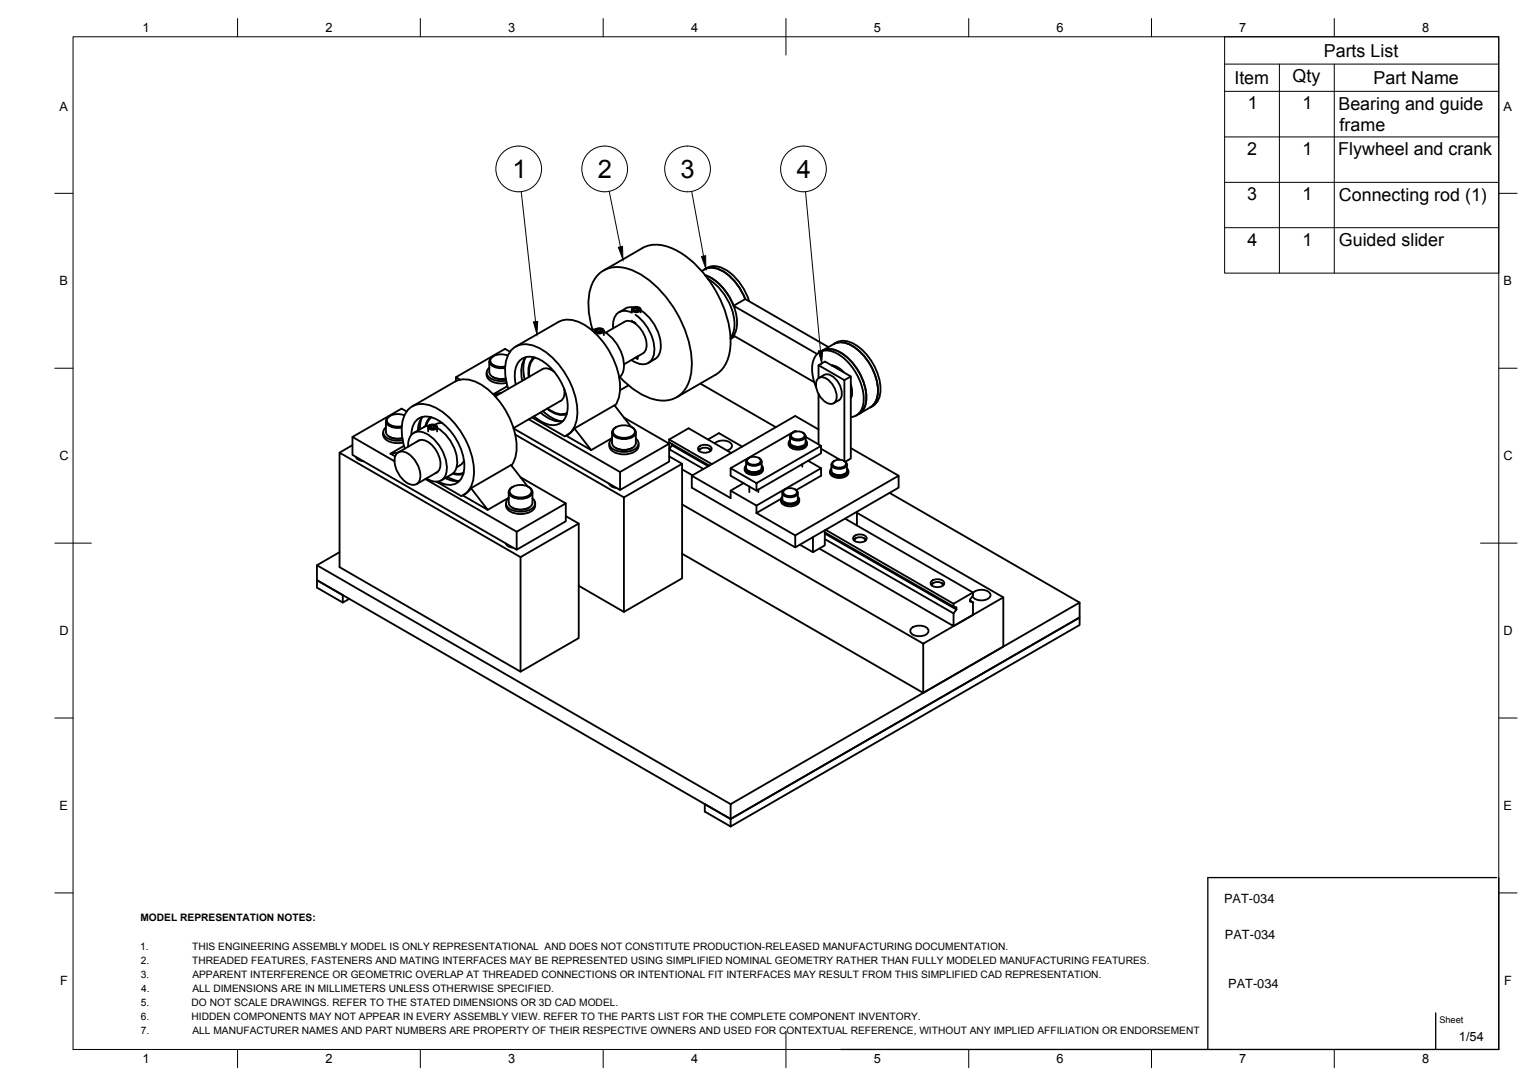
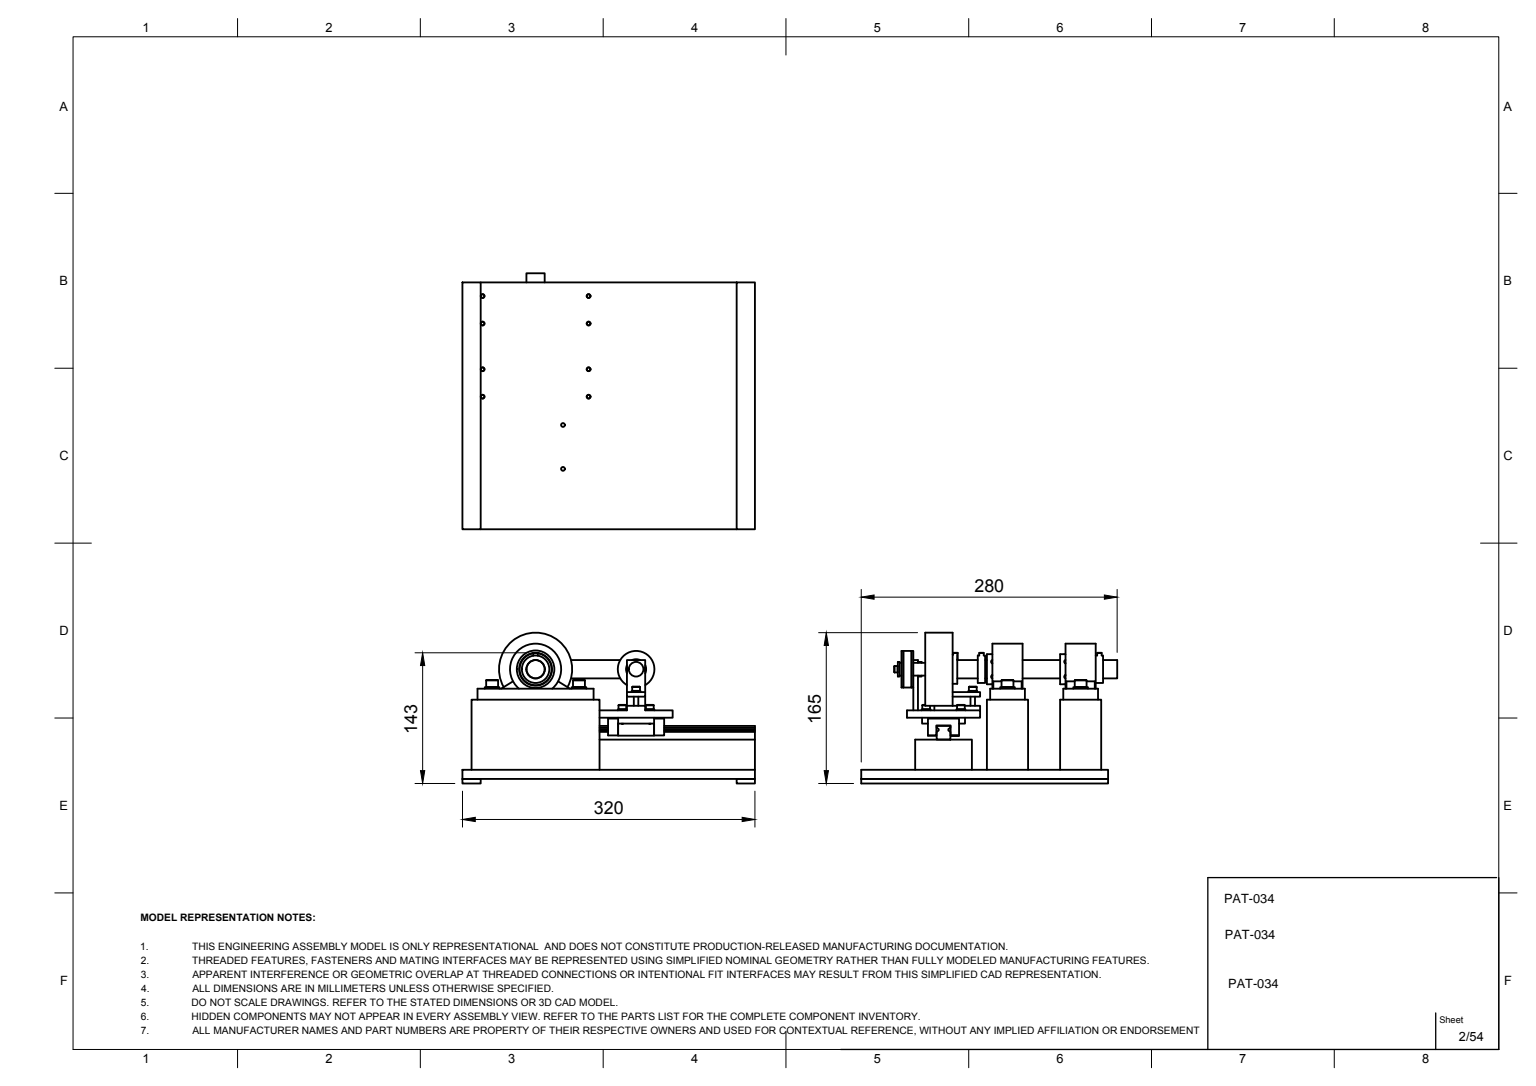
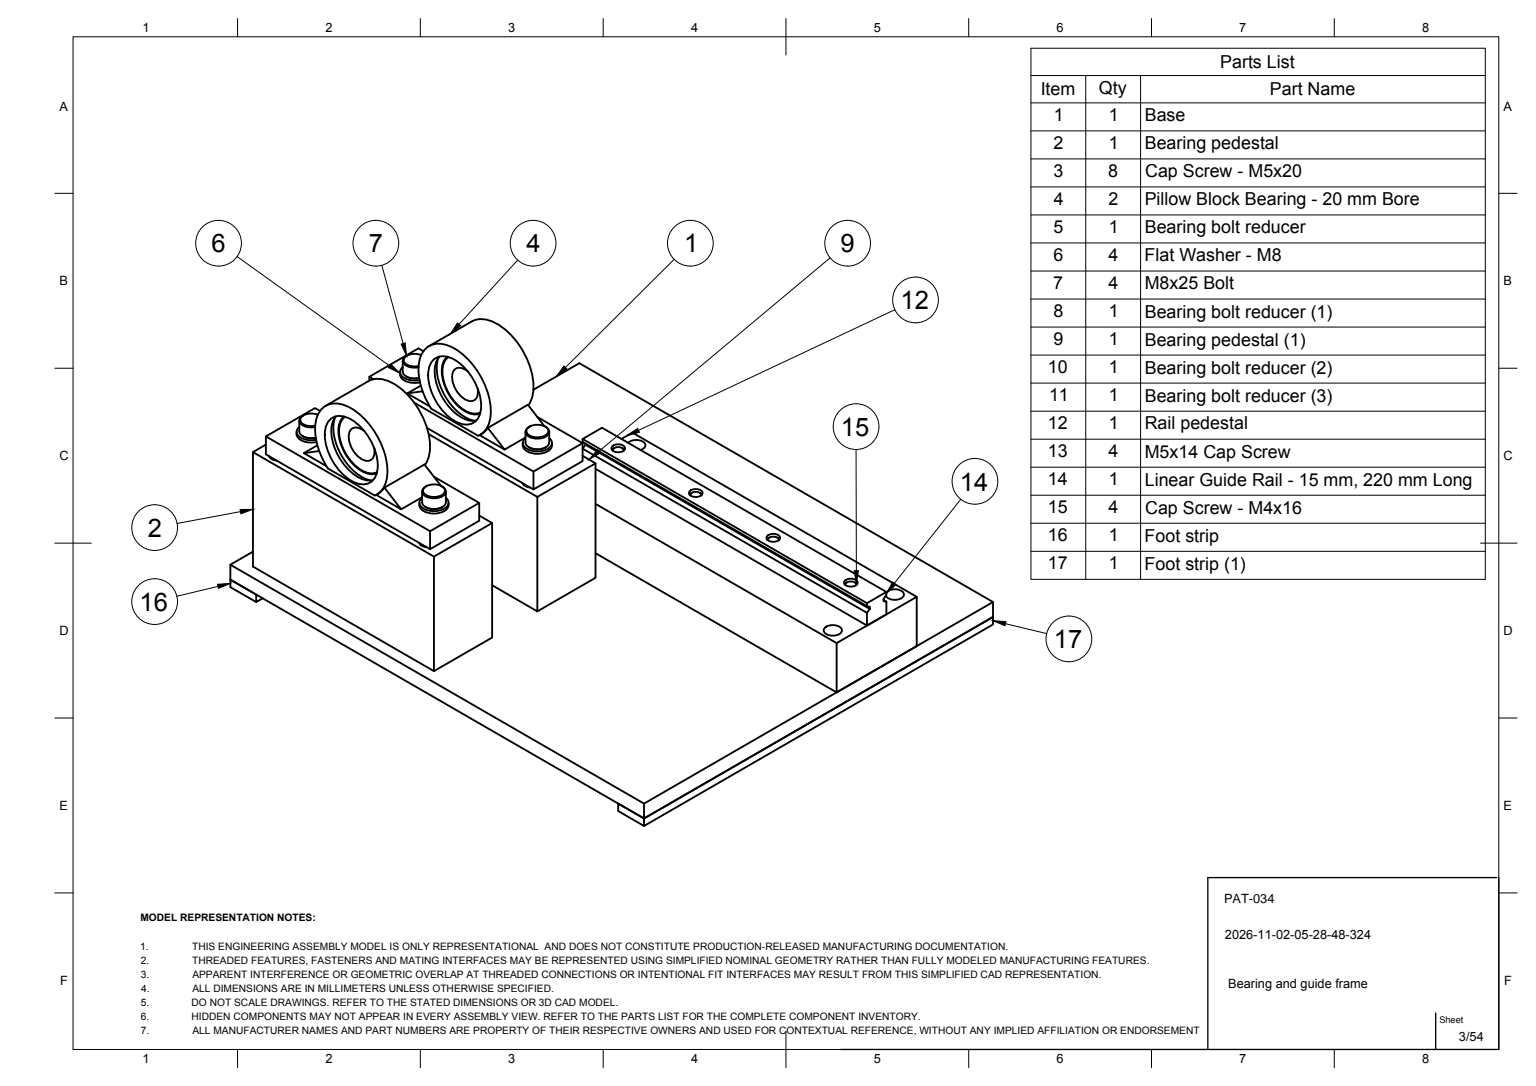
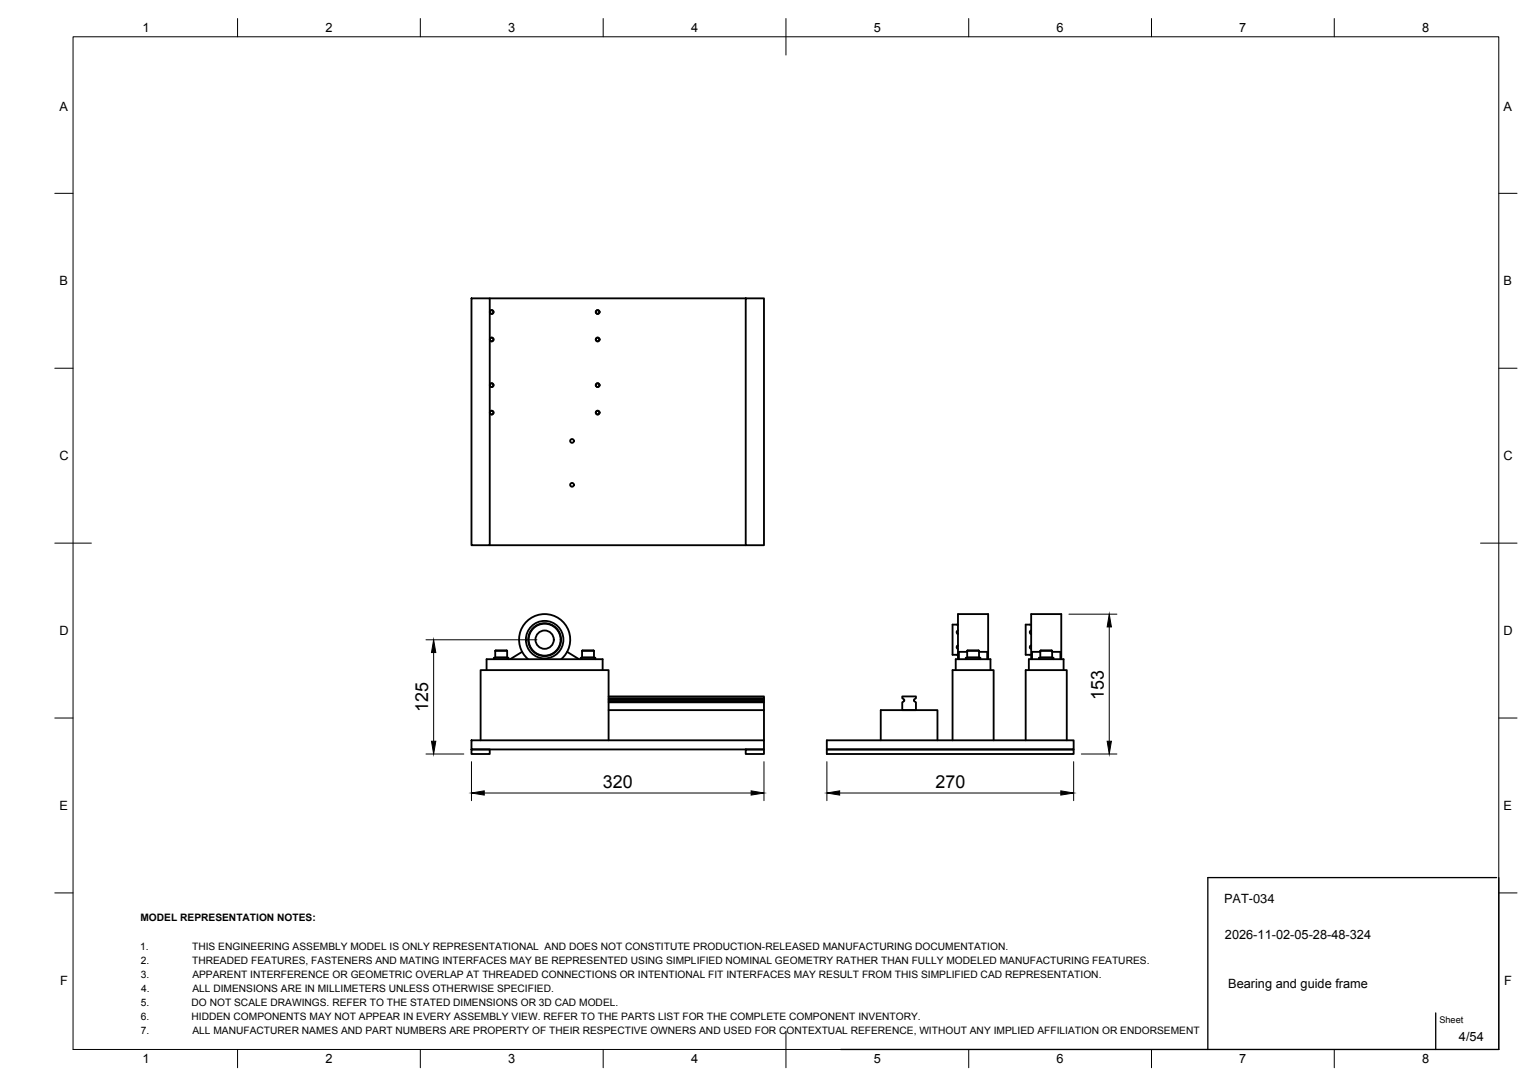
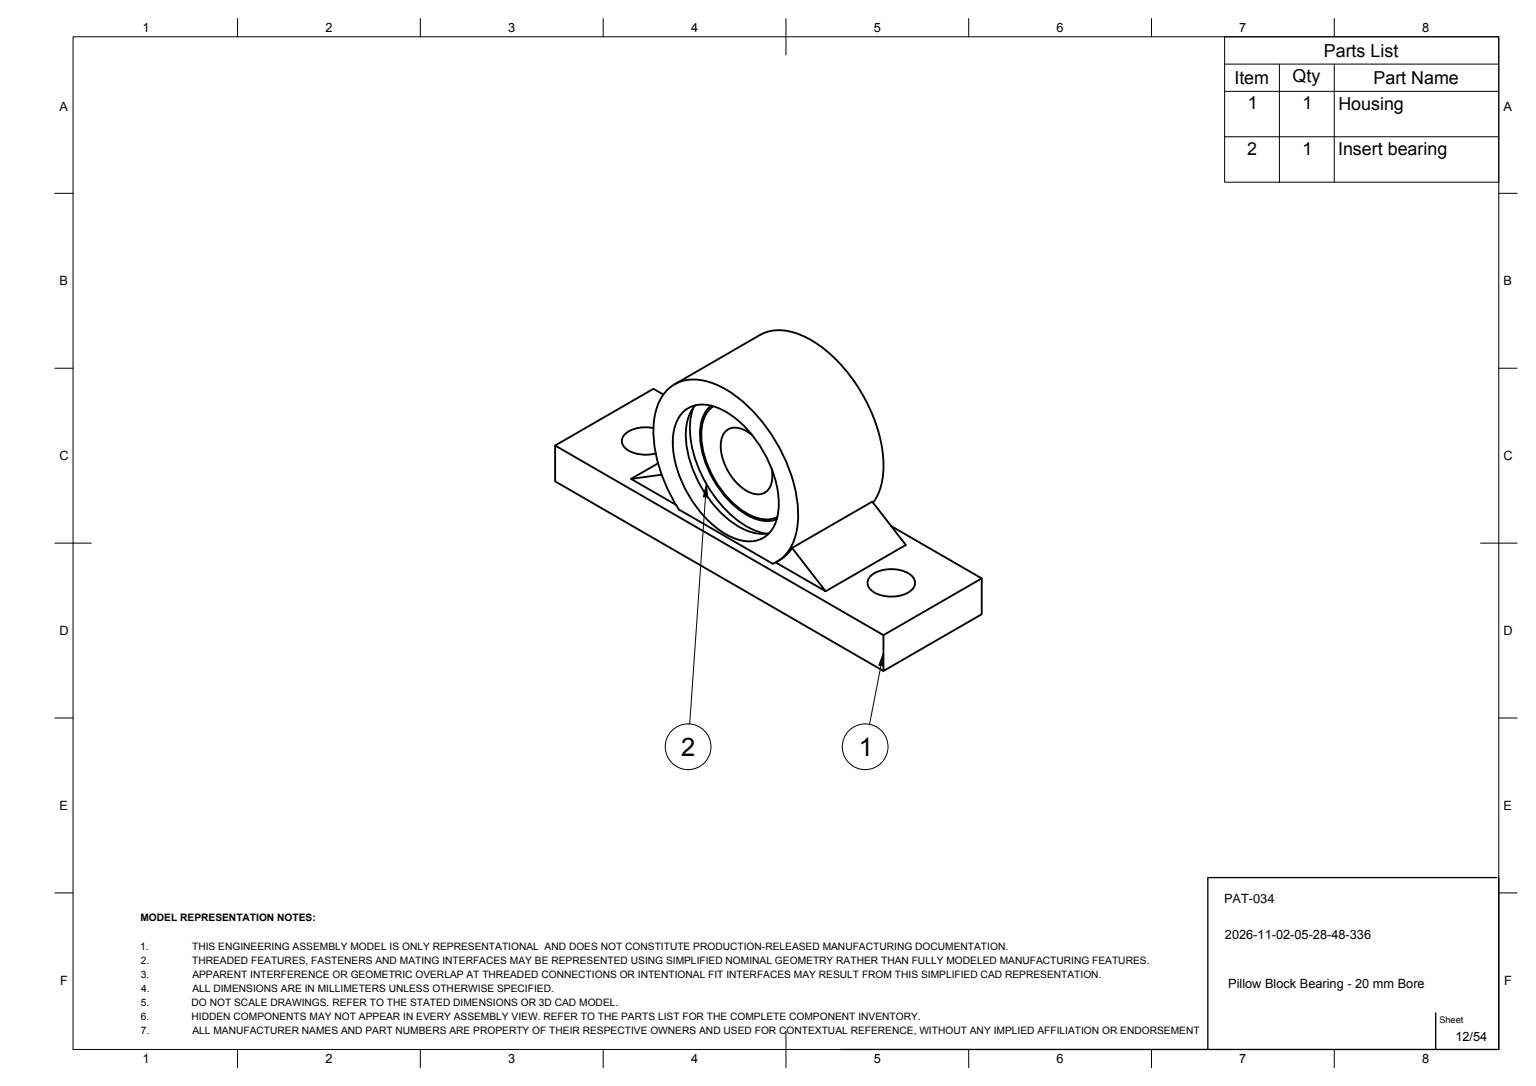
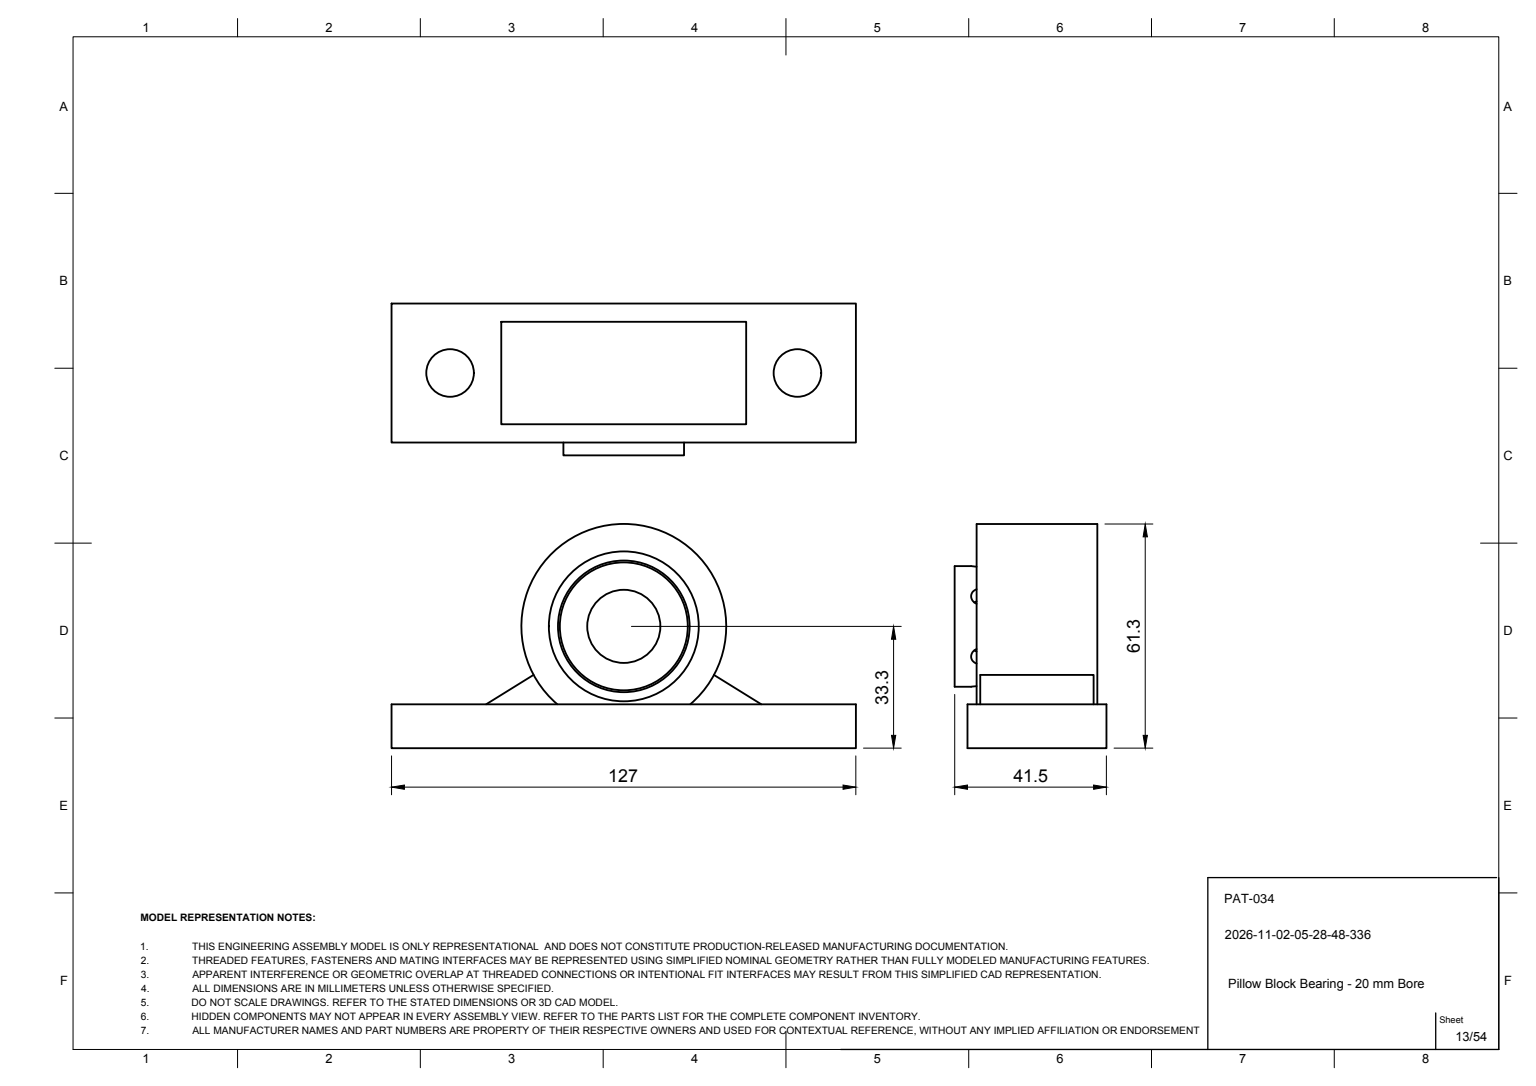
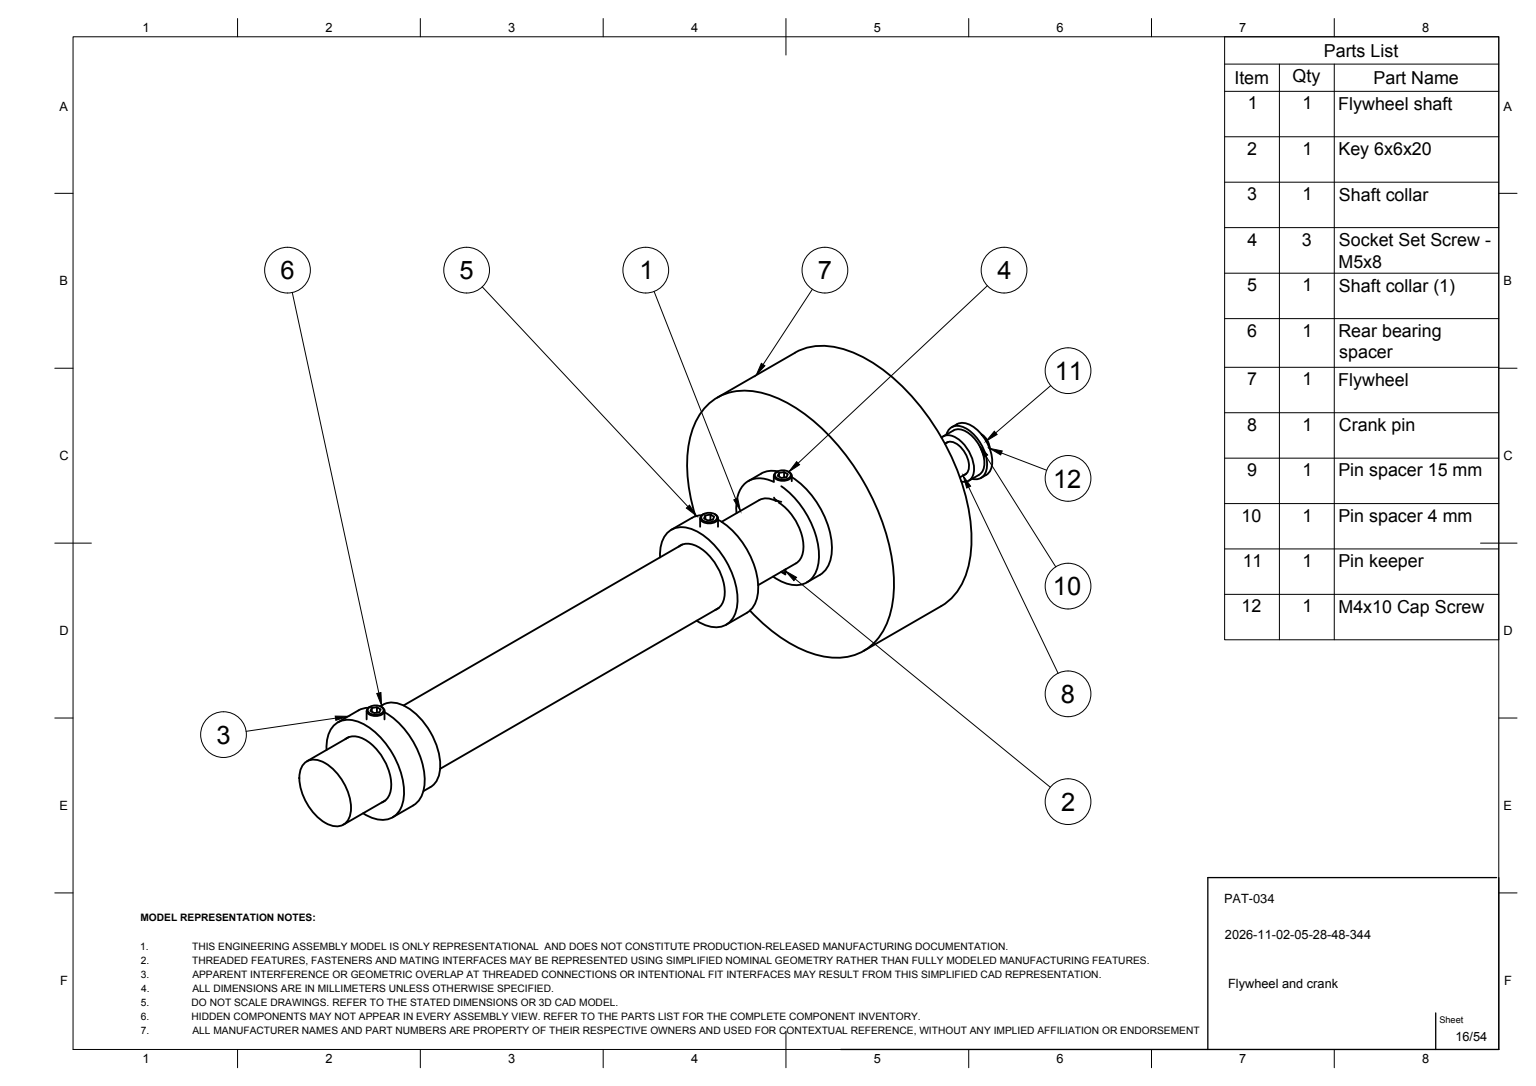
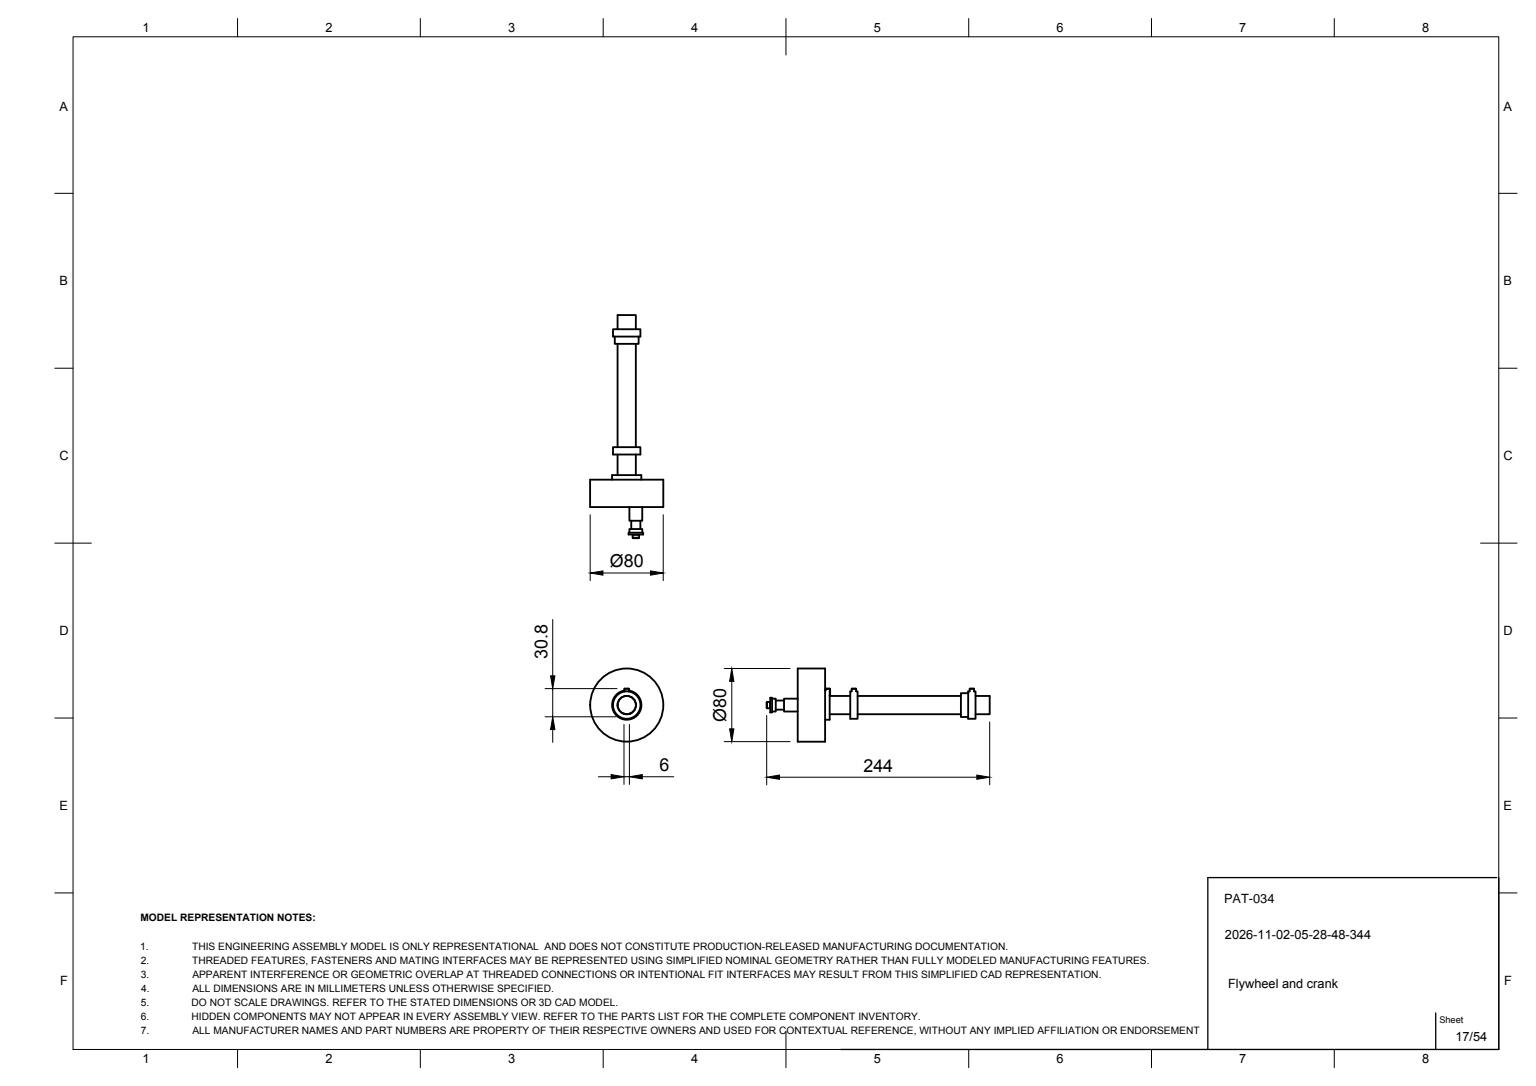
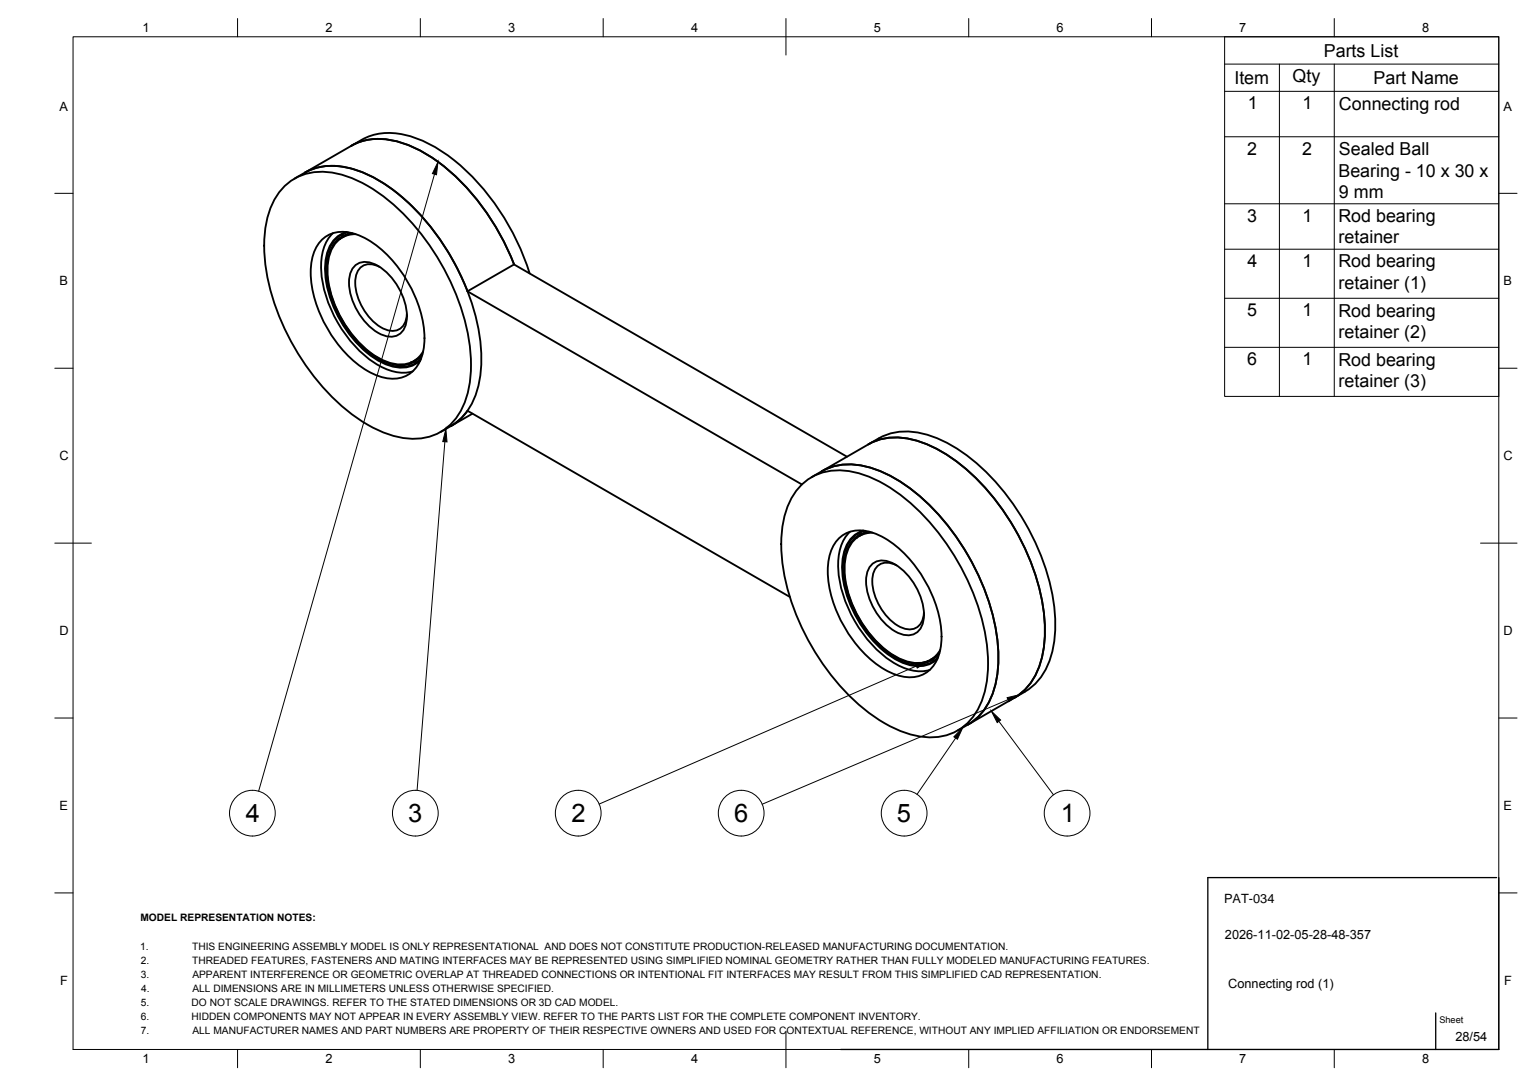
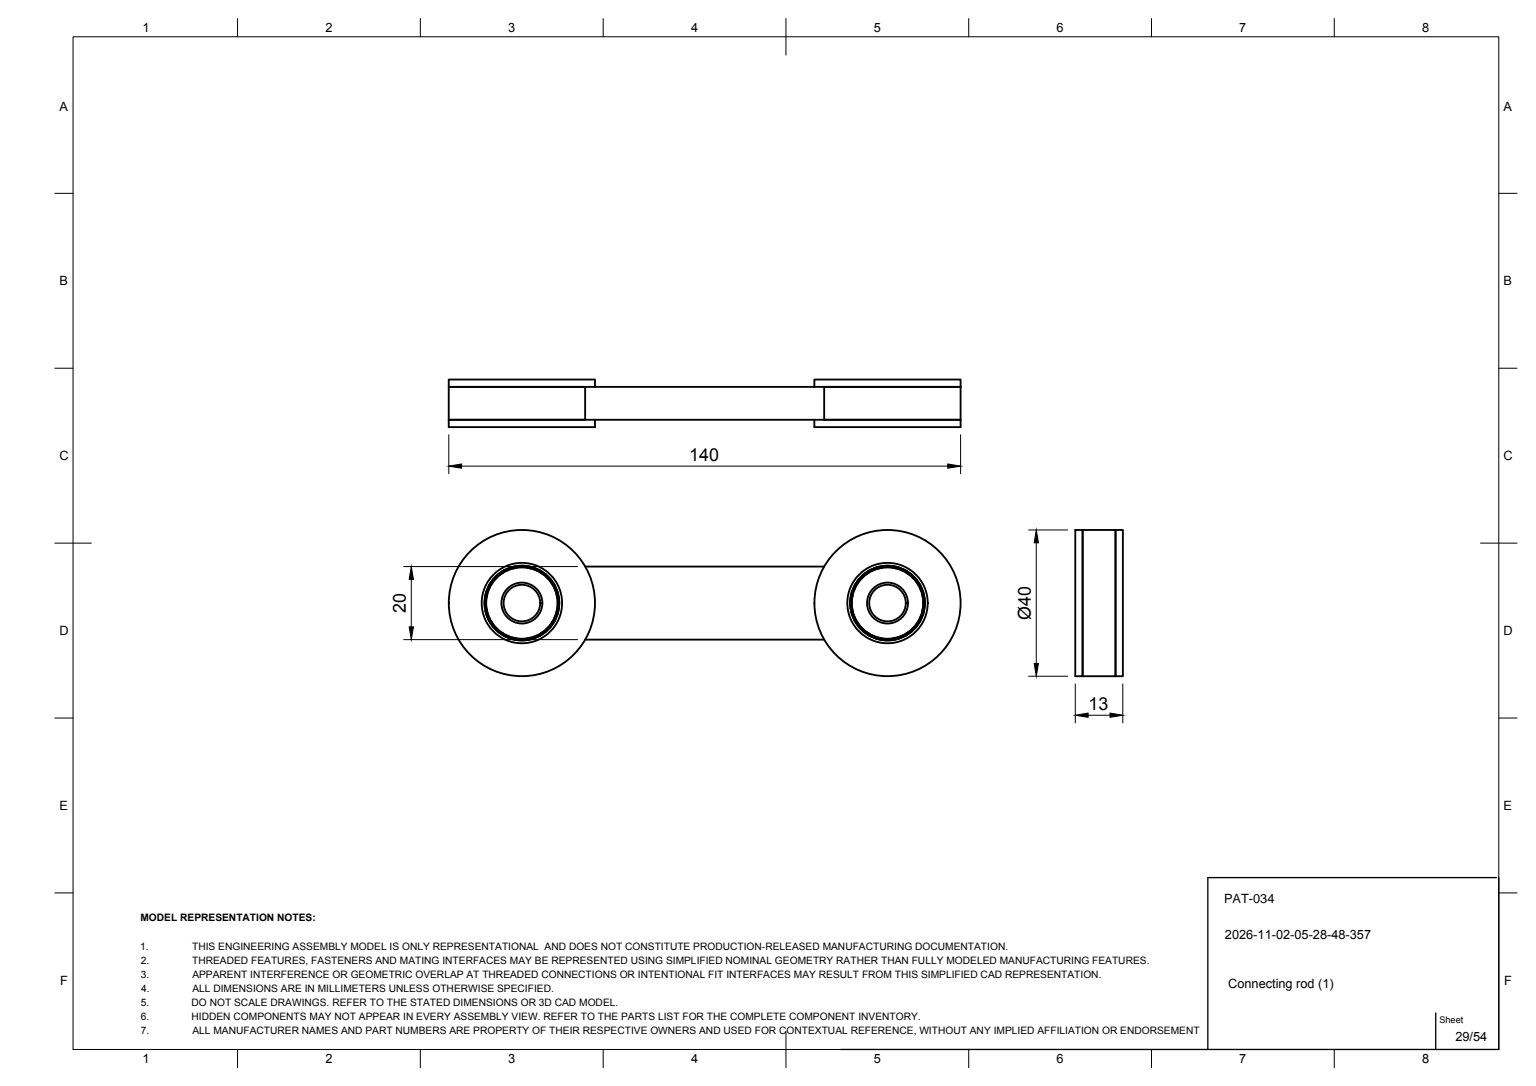
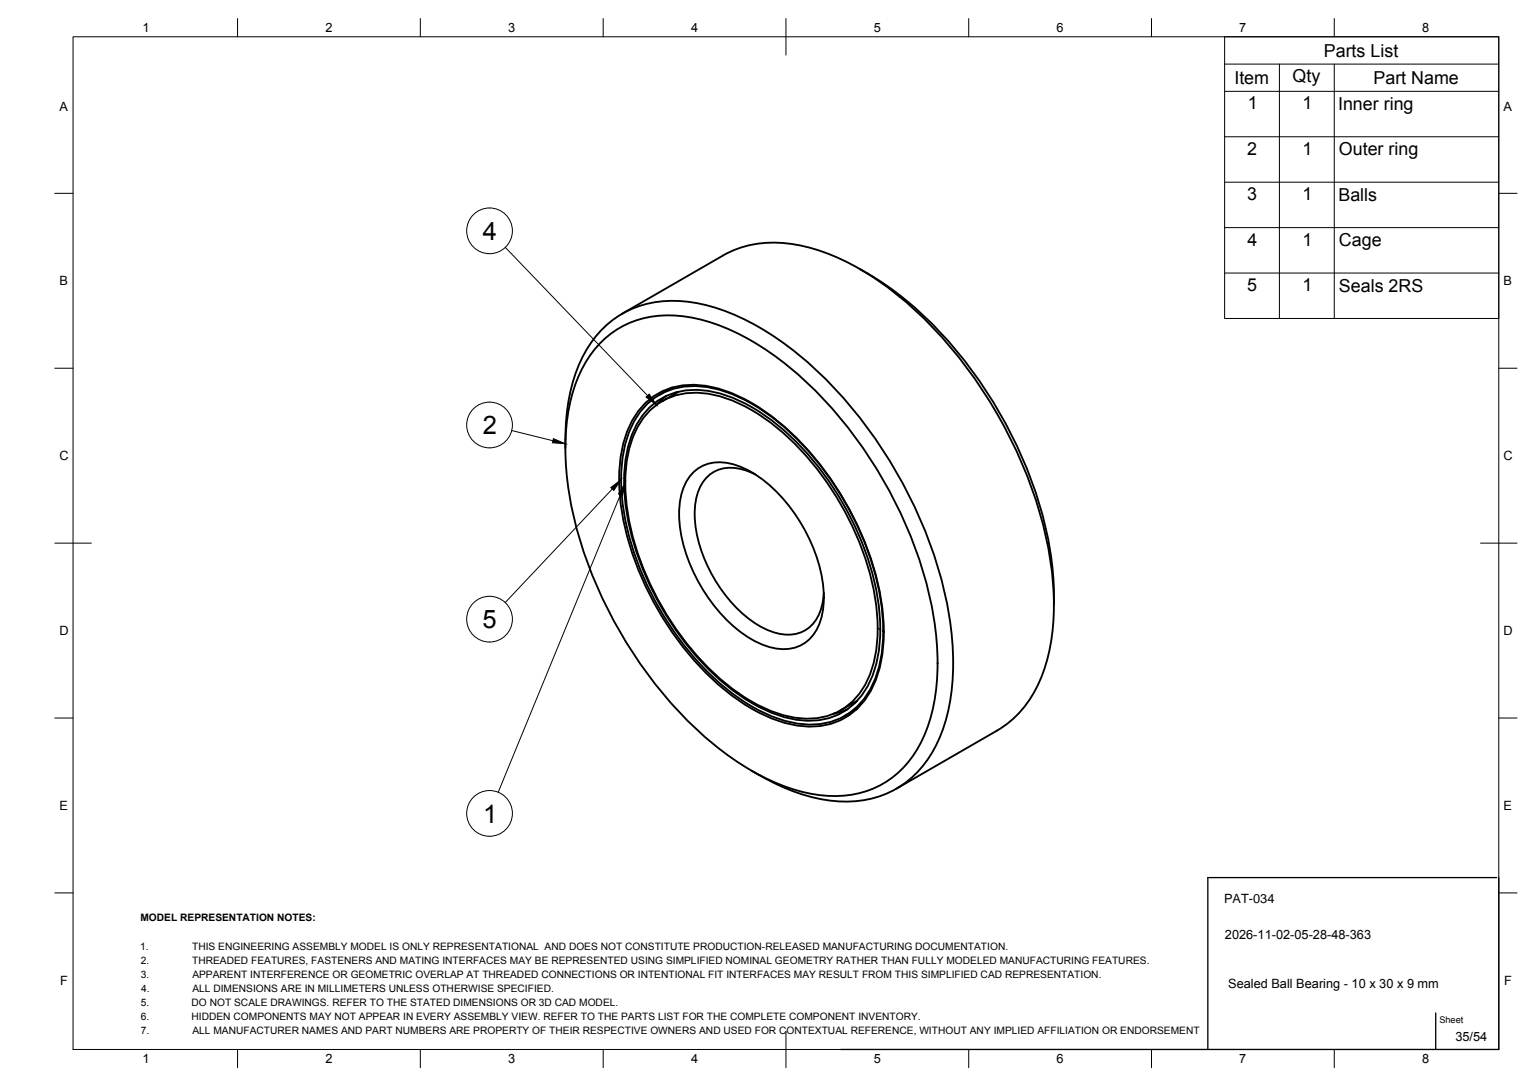
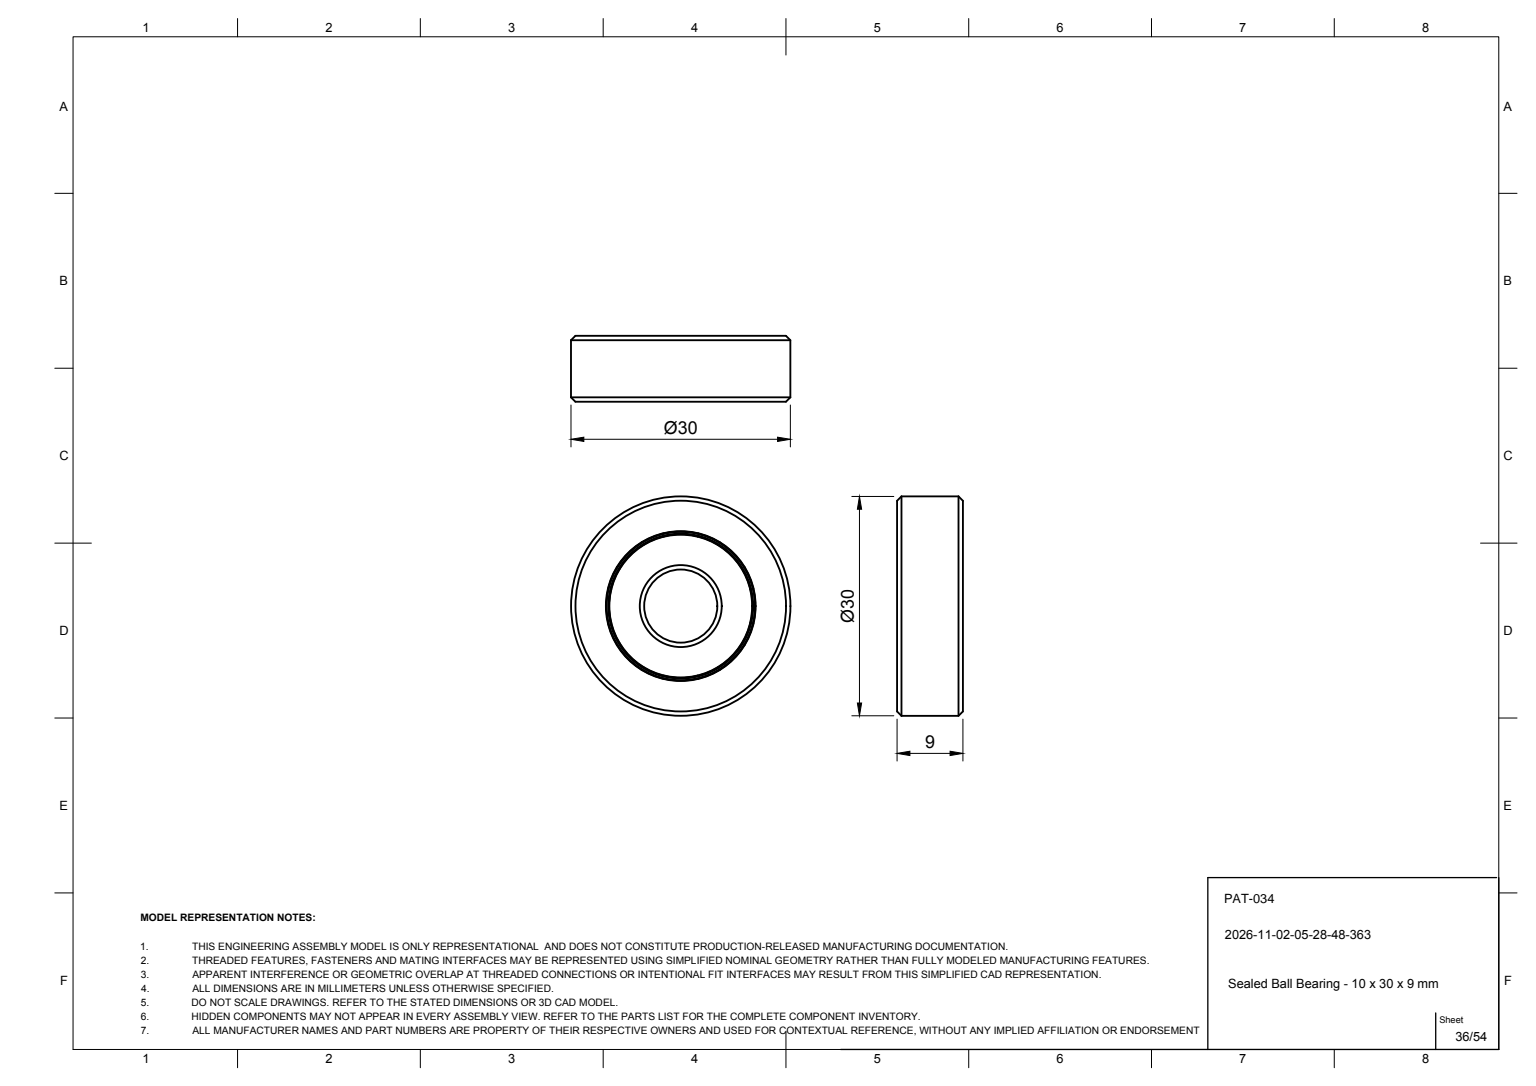
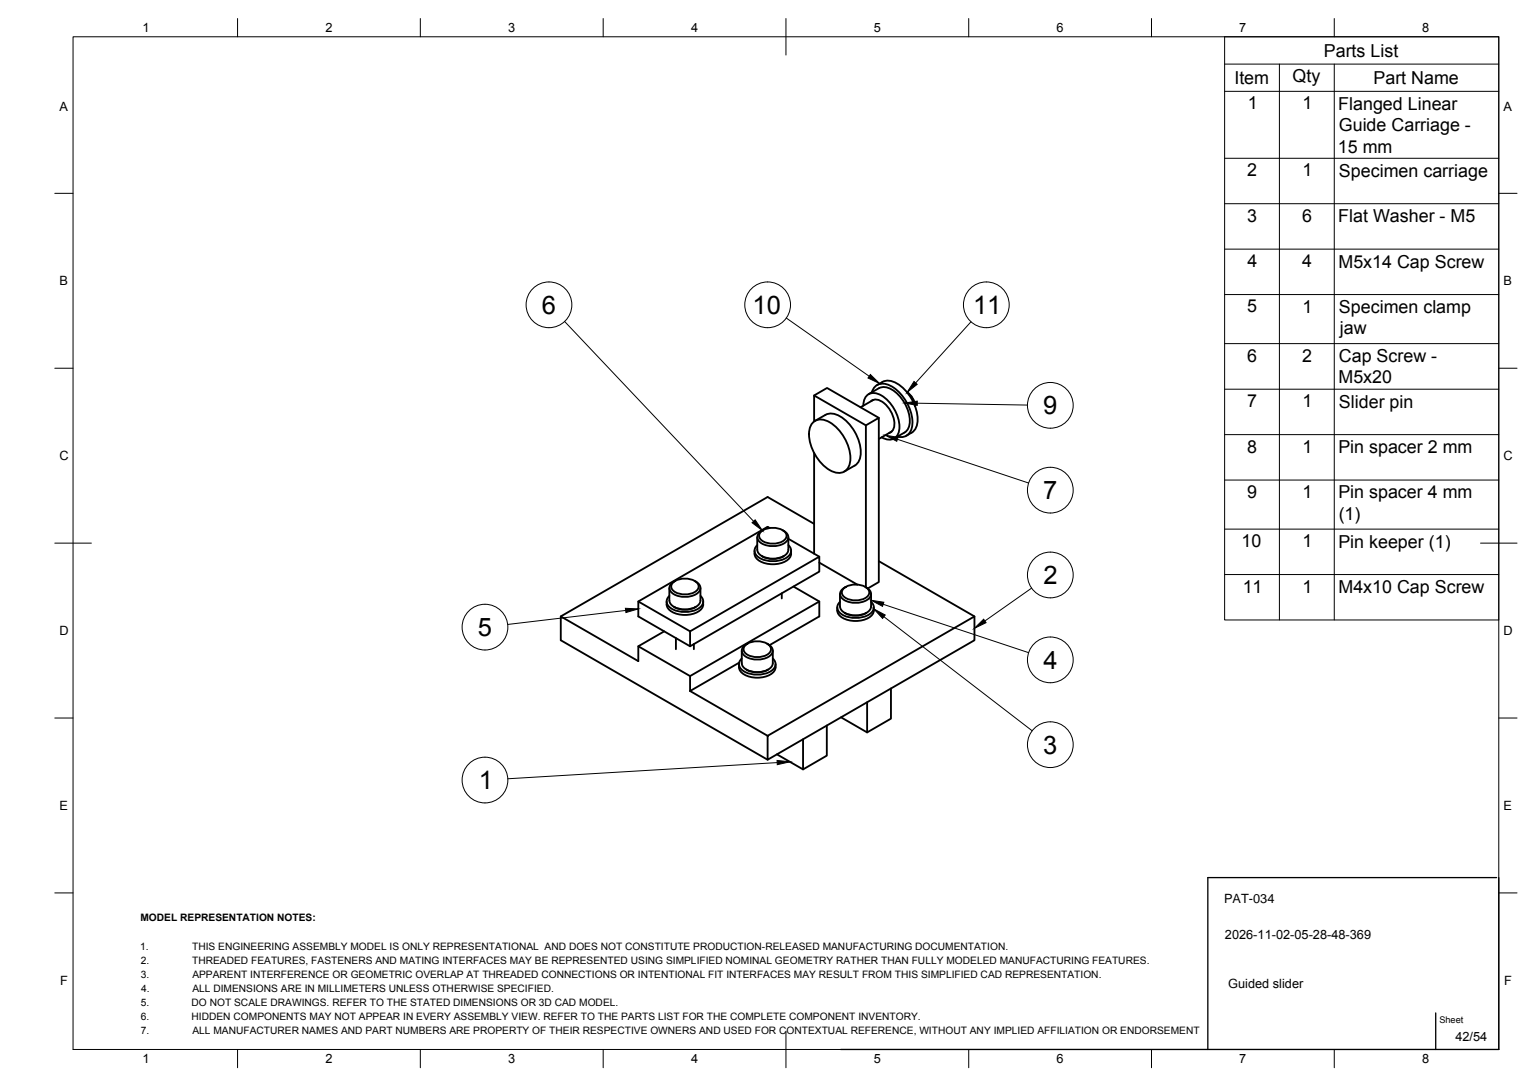
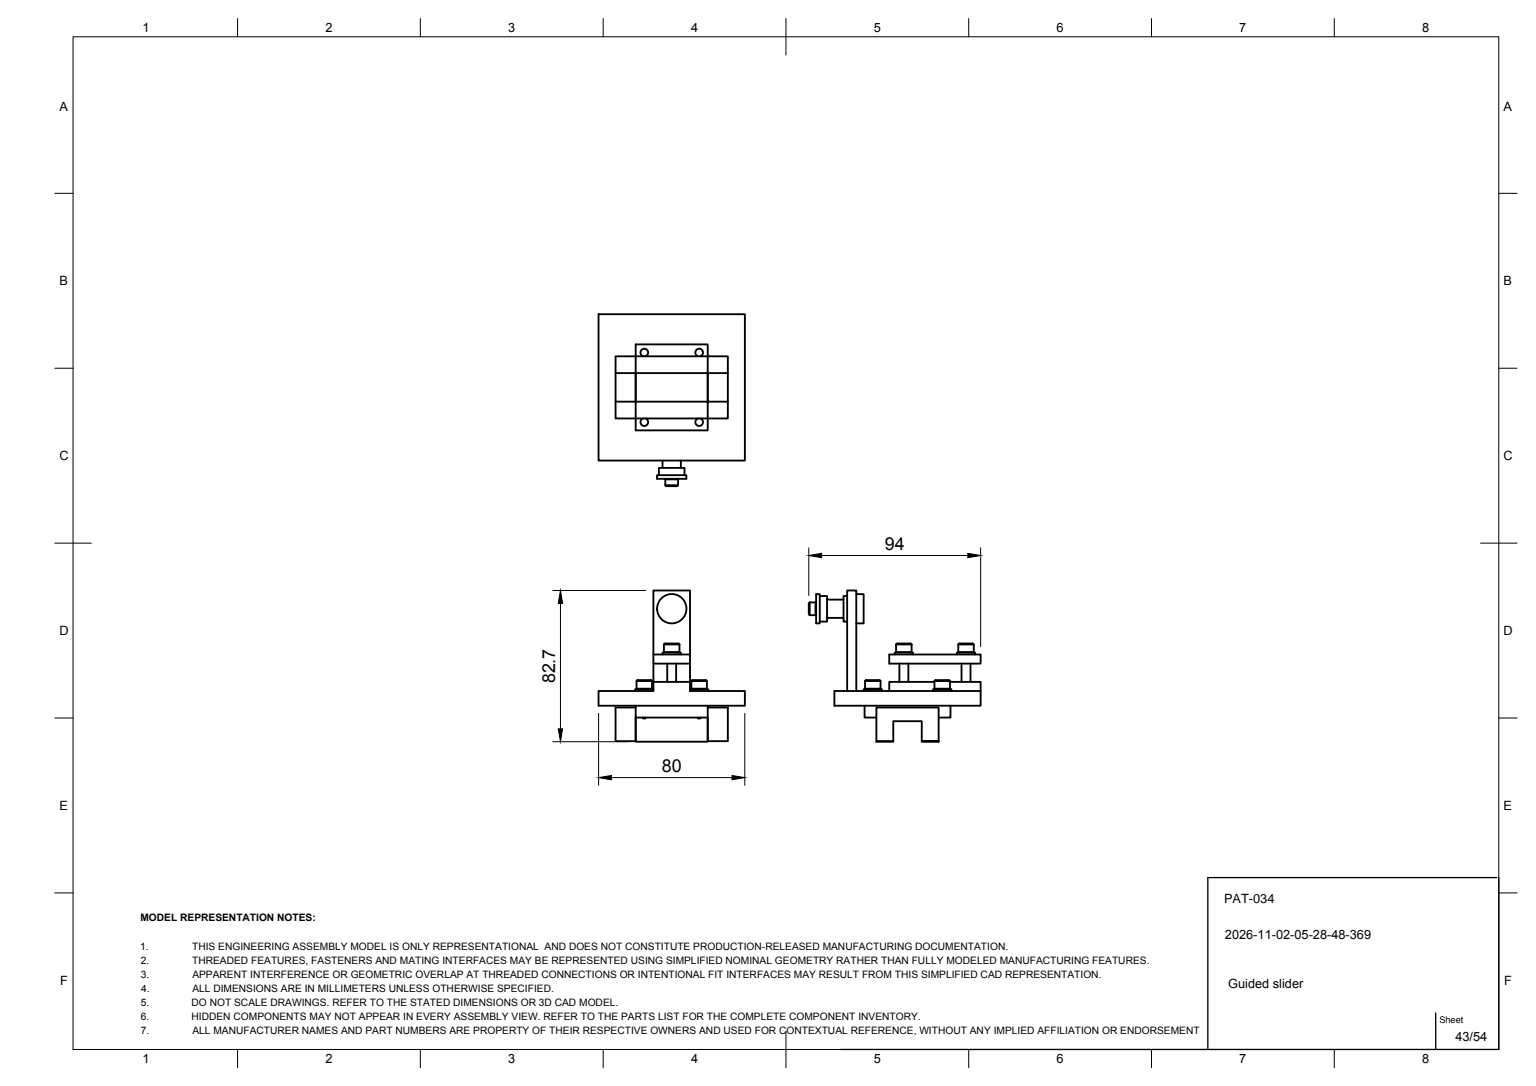
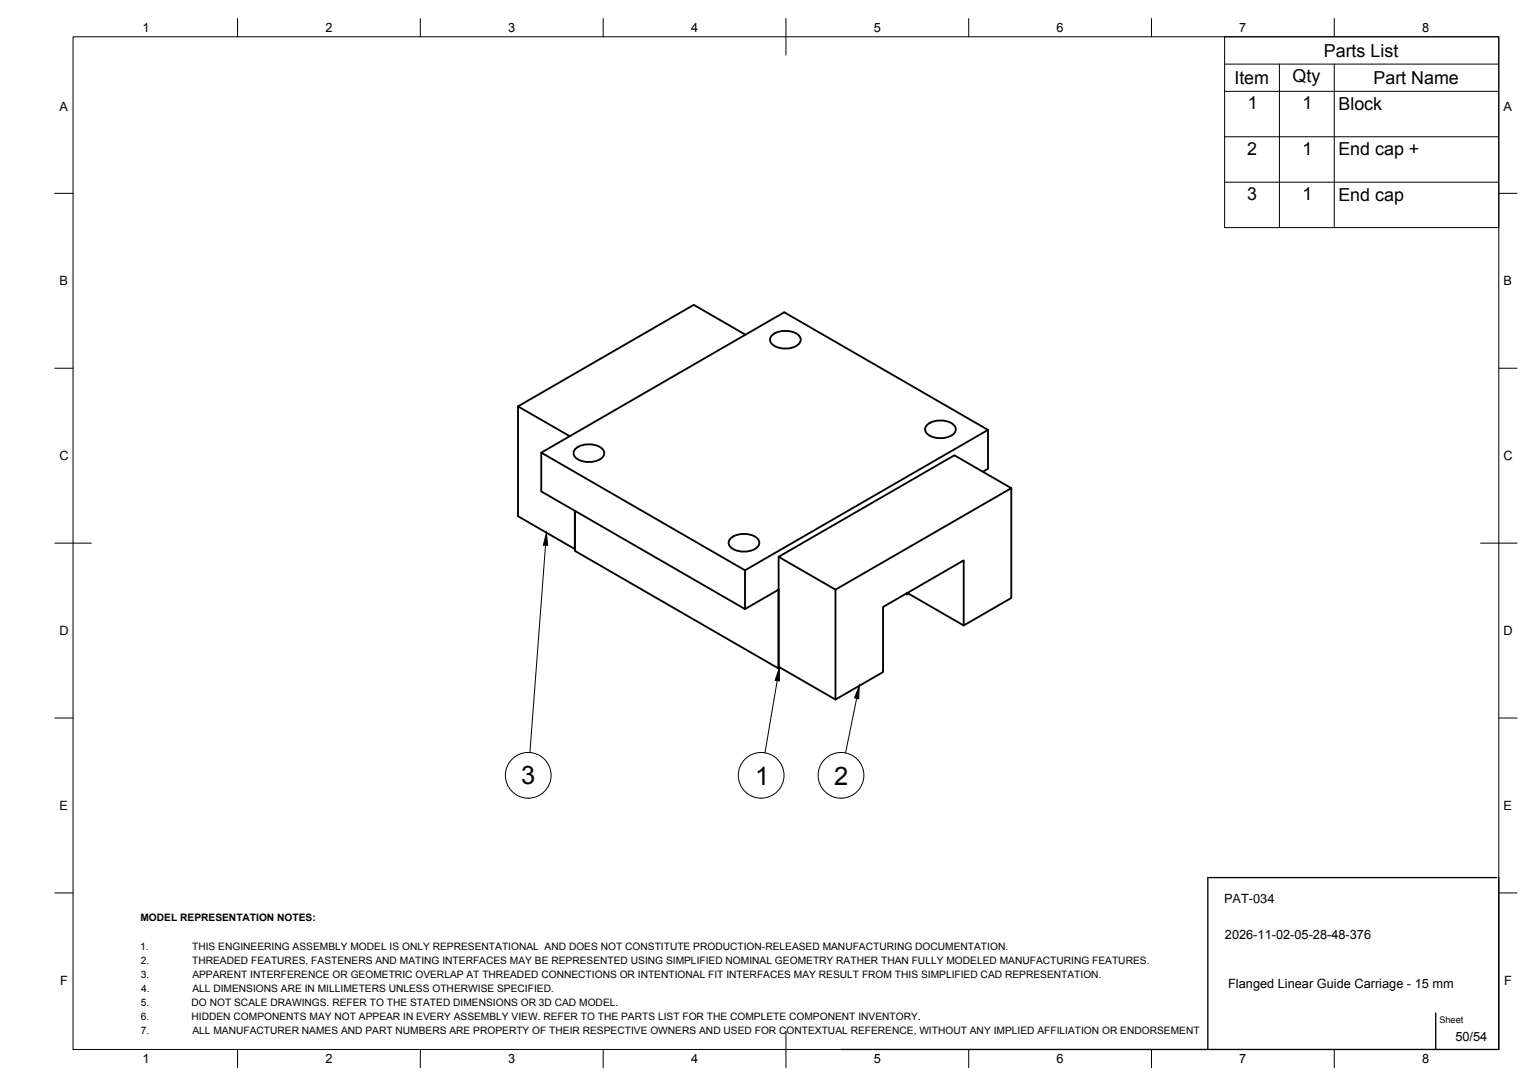
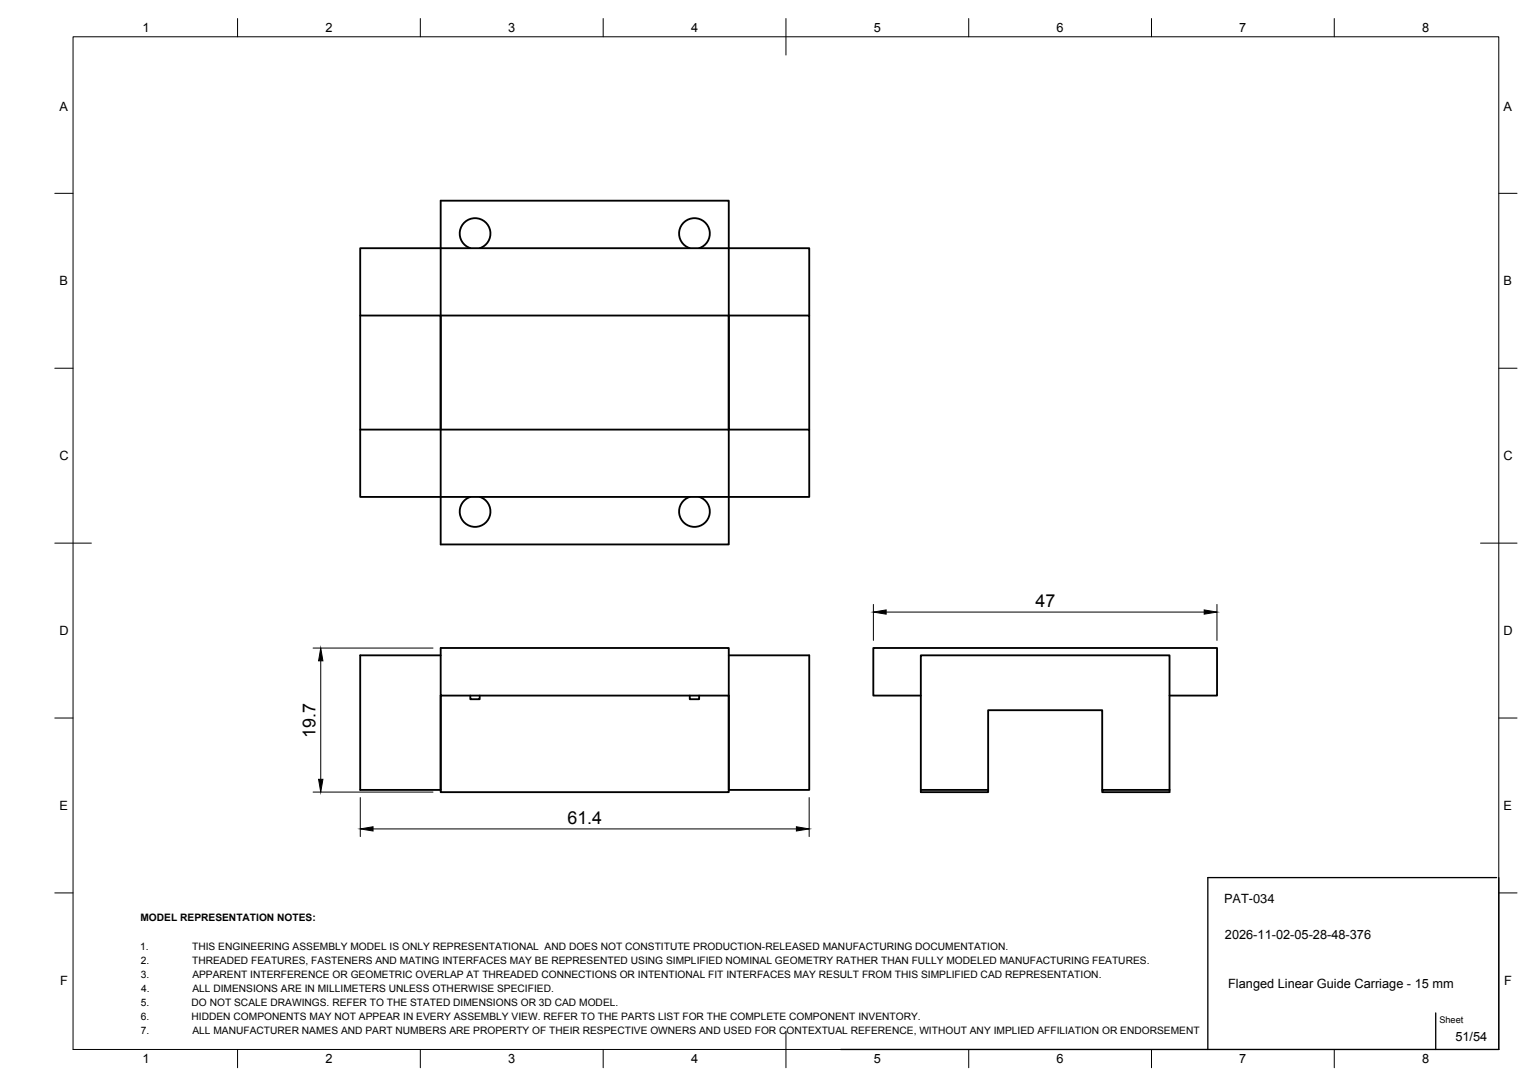
ISO-10303-21;
HEADER;
/* Generated by software containing ST-Developer
 * from STEP Tools, Inc. (www.steptools.com) 
 */

FILE_DESCRIPTION(
/* description */ ('Fatigue rig crank-slider'),
/* implementation_level */ '2;1');

FILE_NAME(
/* name */ 'PAT-034',
/* time_stamp */ '2026-10-28T03:24:50-07:00',
/* author */ (''),
/* organization */ (''),
/* preprocessor_version */ 'ST-DEVELOPER v20.2',
/* originating_system */ 'Autodesk Translation Framework v15.17.0.0',
/* authorisation */ '');

FILE_SCHEMA (('AUTOMOTIVE_DESIGN { 1 0 10303 214 3 1 1 }'));
ENDSEC;

DATA;
#10=MECHANICAL_DESIGN_GEOMETRIC_PRESENTATION_REPRESENTATION('',(#587,#588,
#589,#590,#591,#592,#593,#594,#595,#596,#597,#598,#599,#600,#601,#602,#603,
#604,#605,#606,#607,#608,#609,#610,#611,#612,#613,#614,#615,#616,#617,#618,
#619,#620,#621,#622,#623,#624,#625,#626,#627,#628,#629,#630,#631,#632,#633,
#634,#635,#636,#637,#638,#639,#640,#641,#642,#643,#644,#645),#16911);
#11=TOROIDAL_SURFACE('',#10108,1.,0.247676);
#12=TOROIDAL_SURFACE('',#10128,1.,0.247676);
#13=CONICAL_SURFACE('',#9819,0.625,0.785398163397448);
#14=CONICAL_SURFACE('',#9823,0.635,0.785398163397449);
#15=CONICAL_SURFACE('',#9827,0.41,0.463647609000806);
#16=CONICAL_SURFACE('',#9876,0.325,0.785398163397448);
#17=CONICAL_SURFACE('',#9880,0.335,0.785398163397448);
#18=CONICAL_SURFACE('',#9884,0.21,0.463647609000806);
#19=CONICAL_SURFACE('',#9888,0.18,0.785398163397448);
#20=CONICAL_SURFACE('',#10045,0.235,0.785398163397448);
#21=CONICAL_SURFACE('',#10049,0.2125,0.785398163397448);
#22=CONICAL_SURFACE('',#10119,0.53,0.785398163397448);
#23=CONICAL_SURFACE('',#10126,0.53,0.785398163397448);
#24=CONICAL_SURFACE('',#10139,1.47,0.785398163397449);
#25=CONICAL_SURFACE('',#10143,1.47,0.785398163397449);
#26=CONICAL_SURFACE('',#10419,0.4,0.785398163397448);
#27=CONICAL_SURFACE('',#10423,0.41,0.785398163397448);
#28=CONICAL_SURFACE('',#10427,0.26,0.463647609000806);
#29=CONICAL_SURFACE('',#10431,0.275,0.785398163397449);
#30=CONICAL_SURFACE('',#10444,0.4,0.785398163397448);
#31=CONICAL_SURFACE('',#10448,0.41,0.785398163397448);
#32=CONICAL_SURFACE('',#10452,0.26,0.463647609000806);
#33=CONICAL_SURFACE('',#10456,0.225,0.785398163397448);
#34=CONICAL_SURFACE('',#10517,0.325,0.785398163397448);
#35=CONICAL_SURFACE('',#10521,0.335,0.785398163397448);
#36=CONICAL_SURFACE('',#10525,0.21,0.463647609000806);
#37=ORIENTED_CLOSED_SHELL('',*,#8892,.F.);
#38=ORIENTED_CLOSED_SHELL('',*,#8896,.F.);
#39=ORIENTED_CLOSED_SHELL('',*,#8935,.F.);
#40=ORIENTED_CLOSED_SHELL('',*,#8939,.F.);
#41=ORIENTED_CLOSED_SHELL('',*,#8940,.F.);
#42=BREP_WITH_VOIDS('Body1',#8893,(#37));
#43=BREP_WITH_VOIDS('Body1',#8895,(#38));
#44=BREP_WITH_VOIDS('Body1',#8936,(#39));
#45=BREP_WITH_VOIDS('Body1',#8938,(#40));
#46=BREP_WITH_VOIDS('Body1',#8941,(#41));
#47=ITEM_DEFINED_TRANSFORMATION($,$,#9726,#9795);
#48=ITEM_DEFINED_TRANSFORMATION($,$,#9767,#9796);
#49=ITEM_DEFINED_TRANSFORMATION($,$,#10107,#10235);
#50=ITEM_DEFINED_TRANSFORMATION($,$,#10127,#10236);
#51=ITEM_DEFINED_TRANSFORMATION($,$,#10147,#10237);
#52=ITEM_DEFINED_TRANSFORMATION($,$,#10164,#10238);
#53=ITEM_DEFINED_TRANSFORMATION($,$,#10218,#10239);
#54=ITEM_DEFINED_TRANSFORMATION($,$,#10053,#10240);
#55=ITEM_DEFINED_TRANSFORMATION($,$,#10070,#10241);
#56=ITEM_DEFINED_TRANSFORMATION($,$,#10079,#10242);
#57=ITEM_DEFINED_TRANSFORMATION($,$,#10088,#10243);
#58=ITEM_DEFINED_TRANSFORMATION($,$,#10097,#10244);
#59=ITEM_DEFINED_TRANSFORMATION($,$,#10106,#10245);
#60=ITEM_DEFINED_TRANSFORMATION($,$,#10106,#10246);
#61=ITEM_DEFINED_TRANSFORMATION($,$,#10342,#10403);
#62=ITEM_DEFINED_TRANSFORMATION($,$,#10381,#10404);
#63=ITEM_DEFINED_TRANSFORMATION($,$,#10392,#10405);
#64=ITEM_DEFINED_TRANSFORMATION($,$,#9495,#10467);
#65=ITEM_DEFINED_TRANSFORMATION($,$,#9538,#10468);
#66=ITEM_DEFINED_TRANSFORMATION($,$,#9581,#10469);
#67=ITEM_DEFINED_TRANSFORMATION($,$,#9590,#10470);
#68=ITEM_DEFINED_TRANSFORMATION($,$,#9599,#10471);
#69=ITEM_DEFINED_TRANSFORMATION($,$,#9642,#10472);
#70=ITEM_DEFINED_TRANSFORMATION($,$,#9651,#10473);
#71=ITEM_DEFINED_TRANSFORMATION($,$,#9660,#10474);
#72=ITEM_DEFINED_TRANSFORMATION($,$,#9711,#10475);
#73=ITEM_DEFINED_TRANSFORMATION($,$,#9718,#10476);
#74=ITEM_DEFINED_TRANSFORMATION($,$,#10441,#10477);
#75=ITEM_DEFINED_TRANSFORMATION($,$,#10441,#10478);
#76=ITEM_DEFINED_TRANSFORMATION($,$,#10441,#10479);
#77=ITEM_DEFINED_TRANSFORMATION($,$,#10441,#10480);
#78=ITEM_DEFINED_TRANSFORMATION($,$,#9725,#10481);
#79=ITEM_DEFINED_TRANSFORMATION($,$,#9797,#10482);
#80=ITEM_DEFINED_TRANSFORMATION($,$,#9806,#10483);
#81=ITEM_DEFINED_TRANSFORMATION($,$,#9797,#10484);
#82=ITEM_DEFINED_TRANSFORMATION($,$,#9806,#10485);
#83=ITEM_DEFINED_TRANSFORMATION($,$,#10441,#10486);
#84=ITEM_DEFINED_TRANSFORMATION($,$,#10441,#10487);
#85=ITEM_DEFINED_TRANSFORMATION($,$,#10441,#10488);
#86=ITEM_DEFINED_TRANSFORMATION($,$,#10441,#10489);
#87=ITEM_DEFINED_TRANSFORMATION($,$,#9725,#10490);
#88=ITEM_DEFINED_TRANSFORMATION($,$,#9797,#10491);
#89=ITEM_DEFINED_TRANSFORMATION($,$,#9806,#10492);
#90=ITEM_DEFINED_TRANSFORMATION($,$,#9797,#10493);
#91=ITEM_DEFINED_TRANSFORMATION($,$,#9806,#10494);
#92=ITEM_DEFINED_TRANSFORMATION($,$,#10406,#10495);
#93=ITEM_DEFINED_TRANSFORMATION($,$,#10406,#10496);
#94=ITEM_DEFINED_TRANSFORMATION($,$,#10406,#10497);
#95=ITEM_DEFINED_TRANSFORMATION($,$,#10406,#10498);
#96=ITEM_DEFINED_TRANSFORMATION($,$,#9830,#10499);
#97=ITEM_DEFINED_TRANSFORMATION($,$,#9873,#10500);
#98=ITEM_DEFINED_TRANSFORMATION($,$,#9873,#10501);
#99=ITEM_DEFINED_TRANSFORMATION($,$,#9873,#10502);
#100=ITEM_DEFINED_TRANSFORMATION($,$,#9873,#10503);
#101=ITEM_DEFINED_TRANSFORMATION($,$,#9900,#10528);
#102=ITEM_DEFINED_TRANSFORMATION($,$,#9912,#10529);
#103=ITEM_DEFINED_TRANSFORMATION($,$,#9927,#10530);
#104=ITEM_DEFINED_TRANSFORMATION($,$,#9942,#10531);
#105=ITEM_DEFINED_TRANSFORMATION($,$,#9951,#10532);
#106=ITEM_DEFINED_TRANSFORMATION($,$,#9983,#10533);
#107=ITEM_DEFINED_TRANSFORMATION($,$,#9997,#10534);
#108=ITEM_DEFINED_TRANSFORMATION($,$,#10006,#10535);
#109=ITEM_DEFINED_TRANSFORMATION($,$,#10015,#10536);
#110=ITEM_DEFINED_TRANSFORMATION($,$,#10024,#10537);
#111=ITEM_DEFINED_TRANSFORMATION($,$,#10035,#10538);
#112=ITEM_DEFINED_TRANSFORMATION($,$,#10035,#10539);
#113=ITEM_DEFINED_TRANSFORMATION($,$,#10035,#10540);
#114=ITEM_DEFINED_TRANSFORMATION($,$,#10504,#10541);
#115=ITEM_DEFINED_TRANSFORMATION($,$,#10248,#10542);
#116=ITEM_DEFINED_TRANSFORMATION($,$,#10287,#10543);
#117=ITEM_DEFINED_TRANSFORMATION($,$,#10300,#10544);
#118=ITEM_DEFINED_TRANSFORMATION($,$,#10314,#10545);
#119=ITEM_DEFINED_TRANSFORMATION($,$,#10323,#10546);
#120=ITEM_DEFINED_TRANSFORMATION($,$,#10332,#10547);
#121=ITEM_DEFINED_TRANSFORMATION($,$,#10341,#10548);
#122=ITEM_DEFINED_TRANSFORMATION($,$,#10430,#10549);
#123=ITEM_DEFINED_TRANSFORMATION($,$,#10406,#10550);
#124=ITEM_DEFINED_TRANSFORMATION($,$,#10430,#10551);
#125=ITEM_DEFINED_TRANSFORMATION($,$,#10406,#10552);
#126=ITEM_DEFINED_TRANSFORMATION($,$,#10430,#10553);
#127=ITEM_DEFINED_TRANSFORMATION($,$,#10406,#10554);
#128=ITEM_DEFINED_TRANSFORMATION($,$,#10430,#10555);
#129=ITEM_DEFINED_TRANSFORMATION($,$,#10406,#10556);
#130=ITEM_DEFINED_TRANSFORMATION($,$,#10430,#10557);
#131=ITEM_DEFINED_TRANSFORMATION($,$,#10441,#10558);
#132=ITEM_DEFINED_TRANSFORMATION($,$,#10430,#10559);
#133=ITEM_DEFINED_TRANSFORMATION($,$,#10441,#10560);
#134=ITEM_DEFINED_TRANSFORMATION($,$,#10504,#10561);
#135=ITEM_DEFINED_TRANSFORMATION($,$,#9494,#10562);
#136=ITEM_DEFINED_TRANSFORMATION($,$,#9899,#10563);
#137=ITEM_DEFINED_TRANSFORMATION($,$,#10052,#10564);
#138=ITEM_DEFINED_TRANSFORMATION($,$,#10247,#10565);
#139=(
REPRESENTATION_RELATIONSHIP($,$,#17137,#17136)
REPRESENTATION_RELATIONSHIP_WITH_TRANSFORMATION(#47)
SHAPE_REPRESENTATION_RELATIONSHIP()
);
#140=(
REPRESENTATION_RELATIONSHIP($,$,#17138,#17136)
REPRESENTATION_RELATIONSHIP_WITH_TRANSFORMATION(#48)
SHAPE_REPRESENTATION_RELATIONSHIP()
);
#141=(
REPRESENTATION_RELATIONSHIP($,$,#17162,#17161)
REPRESENTATION_RELATIONSHIP_WITH_TRANSFORMATION(#49)
SHAPE_REPRESENTATION_RELATIONSHIP()
);
#142=(
REPRESENTATION_RELATIONSHIP($,$,#17163,#17161)
REPRESENTATION_RELATIONSHIP_WITH_TRANSFORMATION(#50)
SHAPE_REPRESENTATION_RELATIONSHIP()
);
#143=(
REPRESENTATION_RELATIONSHIP($,$,#17164,#17161)
REPRESENTATION_RELATIONSHIP_WITH_TRANSFORMATION(#51)
SHAPE_REPRESENTATION_RELATIONSHIP()
);
#144=(
REPRESENTATION_RELATIONSHIP($,$,#17165,#17161)
REPRESENTATION_RELATIONSHIP_WITH_TRANSFORMATION(#52)
SHAPE_REPRESENTATION_RELATIONSHIP()
);
#145=(
REPRESENTATION_RELATIONSHIP($,$,#17166,#17161)
REPRESENTATION_RELATIONSHIP_WITH_TRANSFORMATION(#53)
SHAPE_REPRESENTATION_RELATIONSHIP()
);
#146=(
REPRESENTATION_RELATIONSHIP($,$,#17156,#17155)
REPRESENTATION_RELATIONSHIP_WITH_TRANSFORMATION(#54)
SHAPE_REPRESENTATION_RELATIONSHIP()
);
#147=(
REPRESENTATION_RELATIONSHIP($,$,#17157,#17155)
REPRESENTATION_RELATIONSHIP_WITH_TRANSFORMATION(#55)
SHAPE_REPRESENTATION_RELATIONSHIP()
);
#148=(
REPRESENTATION_RELATIONSHIP($,$,#17158,#17155)
REPRESENTATION_RELATIONSHIP_WITH_TRANSFORMATION(#56)
SHAPE_REPRESENTATION_RELATIONSHIP()
);
#149=(
REPRESENTATION_RELATIONSHIP($,$,#17159,#17155)
REPRESENTATION_RELATIONSHIP_WITH_TRANSFORMATION(#57)
SHAPE_REPRESENTATION_RELATIONSHIP()
);
#150=(
REPRESENTATION_RELATIONSHIP($,$,#17160,#17155)
REPRESENTATION_RELATIONSHIP_WITH_TRANSFORMATION(#58)
SHAPE_REPRESENTATION_RELATIONSHIP()
);
#151=(
REPRESENTATION_RELATIONSHIP($,$,#17161,#17155)
REPRESENTATION_RELATIONSHIP_WITH_TRANSFORMATION(#59)
SHAPE_REPRESENTATION_RELATIONSHIP()
);
#152=(
REPRESENTATION_RELATIONSHIP($,$,#17161,#17155)
REPRESENTATION_RELATIONSHIP_WITH_TRANSFORMATION(#60)
SHAPE_REPRESENTATION_RELATIONSHIP()
);
#153=(
REPRESENTATION_RELATIONSHIP($,$,#17175,#17174)
REPRESENTATION_RELATIONSHIP_WITH_TRANSFORMATION(#61)
SHAPE_REPRESENTATION_RELATIONSHIP()
);
#154=(
REPRESENTATION_RELATIONSHIP($,$,#17176,#17174)
REPRESENTATION_RELATIONSHIP_WITH_TRANSFORMATION(#62)
SHAPE_REPRESENTATION_RELATIONSHIP()
);
#155=(
REPRESENTATION_RELATIONSHIP($,$,#17177,#17174)
REPRESENTATION_RELATIONSHIP_WITH_TRANSFORMATION(#63)
SHAPE_REPRESENTATION_RELATIONSHIP()
);
#156=(
REPRESENTATION_RELATIONSHIP($,$,#17126,#17125)
REPRESENTATION_RELATIONSHIP_WITH_TRANSFORMATION(#64)
SHAPE_REPRESENTATION_RELATIONSHIP()
);
#157=(
REPRESENTATION_RELATIONSHIP($,$,#17127,#17125)
REPRESENTATION_RELATIONSHIP_WITH_TRANSFORMATION(#65)
SHAPE_REPRESENTATION_RELATIONSHIP()
);
#158=(
REPRESENTATION_RELATIONSHIP($,$,#17128,#17125)
REPRESENTATION_RELATIONSHIP_WITH_TRANSFORMATION(#66)
SHAPE_REPRESENTATION_RELATIONSHIP()
);
#159=(
REPRESENTATION_RELATIONSHIP($,$,#17129,#17125)
REPRESENTATION_RELATIONSHIP_WITH_TRANSFORMATION(#67)
SHAPE_REPRESENTATION_RELATIONSHIP()
);
#160=(
REPRESENTATION_RELATIONSHIP($,$,#17130,#17125)
REPRESENTATION_RELATIONSHIP_WITH_TRANSFORMATION(#68)
SHAPE_REPRESENTATION_RELATIONSHIP()
);
#161=(
REPRESENTATION_RELATIONSHIP($,$,#17131,#17125)
REPRESENTATION_RELATIONSHIP_WITH_TRANSFORMATION(#69)
SHAPE_REPRESENTATION_RELATIONSHIP()
);
#162=(
REPRESENTATION_RELATIONSHIP($,$,#17132,#17125)
REPRESENTATION_RELATIONSHIP_WITH_TRANSFORMATION(#70)
SHAPE_REPRESENTATION_RELATIONSHIP()
);
#163=(
REPRESENTATION_RELATIONSHIP($,$,#17133,#17125)
REPRESENTATION_RELATIONSHIP_WITH_TRANSFORMATION(#71)
SHAPE_REPRESENTATION_RELATIONSHIP()
);
#164=(
REPRESENTATION_RELATIONSHIP($,$,#17134,#17125)
REPRESENTATION_RELATIONSHIP_WITH_TRANSFORMATION(#72)
SHAPE_REPRESENTATION_RELATIONSHIP()
);
#165=(
REPRESENTATION_RELATIONSHIP($,$,#17135,#17125)
REPRESENTATION_RELATIONSHIP_WITH_TRANSFORMATION(#73)
SHAPE_REPRESENTATION_RELATIONSHIP()
);
#166=(
REPRESENTATION_RELATIONSHIP($,$,#17180,#17125)
REPRESENTATION_RELATIONSHIP_WITH_TRANSFORMATION(#74)
SHAPE_REPRESENTATION_RELATIONSHIP()
);
#167=(
REPRESENTATION_RELATIONSHIP($,$,#17180,#17125)
REPRESENTATION_RELATIONSHIP_WITH_TRANSFORMATION(#75)
SHAPE_REPRESENTATION_RELATIONSHIP()
);
#168=(
REPRESENTATION_RELATIONSHIP($,$,#17180,#17125)
REPRESENTATION_RELATIONSHIP_WITH_TRANSFORMATION(#76)
SHAPE_REPRESENTATION_RELATIONSHIP()
);
#169=(
REPRESENTATION_RELATIONSHIP($,$,#17180,#17125)
REPRESENTATION_RELATIONSHIP_WITH_TRANSFORMATION(#77)
SHAPE_REPRESENTATION_RELATIONSHIP()
);
#170=(
REPRESENTATION_RELATIONSHIP($,$,#17136,#17125)
REPRESENTATION_RELATIONSHIP_WITH_TRANSFORMATION(#78)
SHAPE_REPRESENTATION_RELATIONSHIP()
);
#171=(
REPRESENTATION_RELATIONSHIP($,$,#17139,#17125)
REPRESENTATION_RELATIONSHIP_WITH_TRANSFORMATION(#79)
SHAPE_REPRESENTATION_RELATIONSHIP()
);
#172=(
REPRESENTATION_RELATIONSHIP($,$,#17140,#17125)
REPRESENTATION_RELATIONSHIP_WITH_TRANSFORMATION(#80)
SHAPE_REPRESENTATION_RELATIONSHIP()
);
#173=(
REPRESENTATION_RELATIONSHIP($,$,#17139,#17125)
REPRESENTATION_RELATIONSHIP_WITH_TRANSFORMATION(#81)
SHAPE_REPRESENTATION_RELATIONSHIP()
);
#174=(
REPRESENTATION_RELATIONSHIP($,$,#17140,#17125)
REPRESENTATION_RELATIONSHIP_WITH_TRANSFORMATION(#82)
SHAPE_REPRESENTATION_RELATIONSHIP()
);
#175=(
REPRESENTATION_RELATIONSHIP($,$,#17180,#17125)
REPRESENTATION_RELATIONSHIP_WITH_TRANSFORMATION(#83)
SHAPE_REPRESENTATION_RELATIONSHIP()
);
#176=(
REPRESENTATION_RELATIONSHIP($,$,#17180,#17125)
REPRESENTATION_RELATIONSHIP_WITH_TRANSFORMATION(#84)
SHAPE_REPRESENTATION_RELATIONSHIP()
);
#177=(
REPRESENTATION_RELATIONSHIP($,$,#17180,#17125)
REPRESENTATION_RELATIONSHIP_WITH_TRANSFORMATION(#85)
SHAPE_REPRESENTATION_RELATIONSHIP()
);
#178=(
REPRESENTATION_RELATIONSHIP($,$,#17180,#17125)
REPRESENTATION_RELATIONSHIP_WITH_TRANSFORMATION(#86)
SHAPE_REPRESENTATION_RELATIONSHIP()
);
#179=(
REPRESENTATION_RELATIONSHIP($,$,#17136,#17125)
REPRESENTATION_RELATIONSHIP_WITH_TRANSFORMATION(#87)
SHAPE_REPRESENTATION_RELATIONSHIP()
);
#180=(
REPRESENTATION_RELATIONSHIP($,$,#17139,#17125)
REPRESENTATION_RELATIONSHIP_WITH_TRANSFORMATION(#88)
SHAPE_REPRESENTATION_RELATIONSHIP()
);
#181=(
REPRESENTATION_RELATIONSHIP($,$,#17140,#17125)
REPRESENTATION_RELATIONSHIP_WITH_TRANSFORMATION(#89)
SHAPE_REPRESENTATION_RELATIONSHIP()
);
#182=(
REPRESENTATION_RELATIONSHIP($,$,#17139,#17125)
REPRESENTATION_RELATIONSHIP_WITH_TRANSFORMATION(#90)
SHAPE_REPRESENTATION_RELATIONSHIP()
);
#183=(
REPRESENTATION_RELATIONSHIP($,$,#17140,#17125)
REPRESENTATION_RELATIONSHIP_WITH_TRANSFORMATION(#91)
SHAPE_REPRESENTATION_RELATIONSHIP()
);
#184=(
REPRESENTATION_RELATIONSHIP($,$,#17178,#17125)
REPRESENTATION_RELATIONSHIP_WITH_TRANSFORMATION(#92)
SHAPE_REPRESENTATION_RELATIONSHIP()
);
#185=(
REPRESENTATION_RELATIONSHIP($,$,#17178,#17125)
REPRESENTATION_RELATIONSHIP_WITH_TRANSFORMATION(#93)
SHAPE_REPRESENTATION_RELATIONSHIP()
);
#186=(
REPRESENTATION_RELATIONSHIP($,$,#17178,#17125)
REPRESENTATION_RELATIONSHIP_WITH_TRANSFORMATION(#94)
SHAPE_REPRESENTATION_RELATIONSHIP()
);
#187=(
REPRESENTATION_RELATIONSHIP($,$,#17178,#17125)
REPRESENTATION_RELATIONSHIP_WITH_TRANSFORMATION(#95)
SHAPE_REPRESENTATION_RELATIONSHIP()
);
#188=(
REPRESENTATION_RELATIONSHIP($,$,#17141,#17125)
REPRESENTATION_RELATIONSHIP_WITH_TRANSFORMATION(#96)
SHAPE_REPRESENTATION_RELATIONSHIP()
);
#189=(
REPRESENTATION_RELATIONSHIP($,$,#17142,#17125)
REPRESENTATION_RELATIONSHIP_WITH_TRANSFORMATION(#97)
SHAPE_REPRESENTATION_RELATIONSHIP()
);
#190=(
REPRESENTATION_RELATIONSHIP($,$,#17142,#17125)
REPRESENTATION_RELATIONSHIP_WITH_TRANSFORMATION(#98)
SHAPE_REPRESENTATION_RELATIONSHIP()
);
#191=(
REPRESENTATION_RELATIONSHIP($,$,#17142,#17125)
REPRESENTATION_RELATIONSHIP_WITH_TRANSFORMATION(#99)
SHAPE_REPRESENTATION_RELATIONSHIP()
);
#192=(
REPRESENTATION_RELATIONSHIP($,$,#17142,#17125)
REPRESENTATION_RELATIONSHIP_WITH_TRANSFORMATION(#100)
SHAPE_REPRESENTATION_RELATIONSHIP()
);
#193=(
REPRESENTATION_RELATIONSHIP($,$,#17144,#17143)
REPRESENTATION_RELATIONSHIP_WITH_TRANSFORMATION(#101)
SHAPE_REPRESENTATION_RELATIONSHIP()
);
#194=(
REPRESENTATION_RELATIONSHIP($,$,#17145,#17143)
REPRESENTATION_RELATIONSHIP_WITH_TRANSFORMATION(#102)
SHAPE_REPRESENTATION_RELATIONSHIP()
);
#195=(
REPRESENTATION_RELATIONSHIP($,$,#17146,#17143)
REPRESENTATION_RELATIONSHIP_WITH_TRANSFORMATION(#103)
SHAPE_REPRESENTATION_RELATIONSHIP()
);
#196=(
REPRESENTATION_RELATIONSHIP($,$,#17147,#17143)
REPRESENTATION_RELATIONSHIP_WITH_TRANSFORMATION(#104)
SHAPE_REPRESENTATION_RELATIONSHIP()
);
#197=(
REPRESENTATION_RELATIONSHIP($,$,#17148,#17143)
REPRESENTATION_RELATIONSHIP_WITH_TRANSFORMATION(#105)
SHAPE_REPRESENTATION_RELATIONSHIP()
);
#198=(
REPRESENTATION_RELATIONSHIP($,$,#17149,#17143)
REPRESENTATION_RELATIONSHIP_WITH_TRANSFORMATION(#106)
SHAPE_REPRESENTATION_RELATIONSHIP()
);
#199=(
REPRESENTATION_RELATIONSHIP($,$,#17150,#17143)
REPRESENTATION_RELATIONSHIP_WITH_TRANSFORMATION(#107)
SHAPE_REPRESENTATION_RELATIONSHIP()
);
#200=(
REPRESENTATION_RELATIONSHIP($,$,#17151,#17143)
REPRESENTATION_RELATIONSHIP_WITH_TRANSFORMATION(#108)
SHAPE_REPRESENTATION_RELATIONSHIP()
);
#201=(
REPRESENTATION_RELATIONSHIP($,$,#17152,#17143)
REPRESENTATION_RELATIONSHIP_WITH_TRANSFORMATION(#109)
SHAPE_REPRESENTATION_RELATIONSHIP()
);
#202=(
REPRESENTATION_RELATIONSHIP($,$,#17153,#17143)
REPRESENTATION_RELATIONSHIP_WITH_TRANSFORMATION(#110)
SHAPE_REPRESENTATION_RELATIONSHIP()
);
#203=(
REPRESENTATION_RELATIONSHIP($,$,#17154,#17143)
REPRESENTATION_RELATIONSHIP_WITH_TRANSFORMATION(#111)
SHAPE_REPRESENTATION_RELATIONSHIP()
);
#204=(
REPRESENTATION_RELATIONSHIP($,$,#17154,#17143)
REPRESENTATION_RELATIONSHIP_WITH_TRANSFORMATION(#112)
SHAPE_REPRESENTATION_RELATIONSHIP()
);
#205=(
REPRESENTATION_RELATIONSHIP($,$,#17154,#17143)
REPRESENTATION_RELATIONSHIP_WITH_TRANSFORMATION(#113)
SHAPE_REPRESENTATION_RELATIONSHIP()
);
#206=(
REPRESENTATION_RELATIONSHIP($,$,#17181,#17143)
REPRESENTATION_RELATIONSHIP_WITH_TRANSFORMATION(#114)
SHAPE_REPRESENTATION_RELATIONSHIP()
);
#207=(
REPRESENTATION_RELATIONSHIP($,$,#17168,#17167)
REPRESENTATION_RELATIONSHIP_WITH_TRANSFORMATION(#115)
SHAPE_REPRESENTATION_RELATIONSHIP()
);
#208=(
REPRESENTATION_RELATIONSHIP($,$,#17169,#17167)
REPRESENTATION_RELATIONSHIP_WITH_TRANSFORMATION(#116)
SHAPE_REPRESENTATION_RELATIONSHIP()
);
#209=(
REPRESENTATION_RELATIONSHIP($,$,#17170,#17167)
REPRESENTATION_RELATIONSHIP_WITH_TRANSFORMATION(#117)
SHAPE_REPRESENTATION_RELATIONSHIP()
);
#210=(
REPRESENTATION_RELATIONSHIP($,$,#17171,#17167)
REPRESENTATION_RELATIONSHIP_WITH_TRANSFORMATION(#118)
SHAPE_REPRESENTATION_RELATIONSHIP()
);
#211=(
REPRESENTATION_RELATIONSHIP($,$,#17172,#17167)
REPRESENTATION_RELATIONSHIP_WITH_TRANSFORMATION(#119)
SHAPE_REPRESENTATION_RELATIONSHIP()
);
#212=(
REPRESENTATION_RELATIONSHIP($,$,#17173,#17167)
REPRESENTATION_RELATIONSHIP_WITH_TRANSFORMATION(#120)
SHAPE_REPRESENTATION_RELATIONSHIP()
);
#213=(
REPRESENTATION_RELATIONSHIP($,$,#17174,#17167)
REPRESENTATION_RELATIONSHIP_WITH_TRANSFORMATION(#121)
SHAPE_REPRESENTATION_RELATIONSHIP()
);
#214=(
REPRESENTATION_RELATIONSHIP($,$,#17179,#17167)
REPRESENTATION_RELATIONSHIP_WITH_TRANSFORMATION(#122)
SHAPE_REPRESENTATION_RELATIONSHIP()
);
#215=(
REPRESENTATION_RELATIONSHIP($,$,#17178,#17167)
REPRESENTATION_RELATIONSHIP_WITH_TRANSFORMATION(#123)
SHAPE_REPRESENTATION_RELATIONSHIP()
);
#216=(
REPRESENTATION_RELATIONSHIP($,$,#17179,#17167)
REPRESENTATION_RELATIONSHIP_WITH_TRANSFORMATION(#124)
SHAPE_REPRESENTATION_RELATIONSHIP()
);
#217=(
REPRESENTATION_RELATIONSHIP($,$,#17178,#17167)
REPRESENTATION_RELATIONSHIP_WITH_TRANSFORMATION(#125)
SHAPE_REPRESENTATION_RELATIONSHIP()
);
#218=(
REPRESENTATION_RELATIONSHIP($,$,#17179,#17167)
REPRESENTATION_RELATIONSHIP_WITH_TRANSFORMATION(#126)
SHAPE_REPRESENTATION_RELATIONSHIP()
);
#219=(
REPRESENTATION_RELATIONSHIP($,$,#17178,#17167)
REPRESENTATION_RELATIONSHIP_WITH_TRANSFORMATION(#127)
SHAPE_REPRESENTATION_RELATIONSHIP()
);
#220=(
REPRESENTATION_RELATIONSHIP($,$,#17179,#17167)
REPRESENTATION_RELATIONSHIP_WITH_TRANSFORMATION(#128)
SHAPE_REPRESENTATION_RELATIONSHIP()
);
#221=(
REPRESENTATION_RELATIONSHIP($,$,#17178,#17167)
REPRESENTATION_RELATIONSHIP_WITH_TRANSFORMATION(#129)
SHAPE_REPRESENTATION_RELATIONSHIP()
);
#222=(
REPRESENTATION_RELATIONSHIP($,$,#17179,#17167)
REPRESENTATION_RELATIONSHIP_WITH_TRANSFORMATION(#130)
SHAPE_REPRESENTATION_RELATIONSHIP()
);
#223=(
REPRESENTATION_RELATIONSHIP($,$,#17180,#17167)
REPRESENTATION_RELATIONSHIP_WITH_TRANSFORMATION(#131)
SHAPE_REPRESENTATION_RELATIONSHIP()
);
#224=(
REPRESENTATION_RELATIONSHIP($,$,#17179,#17167)
REPRESENTATION_RELATIONSHIP_WITH_TRANSFORMATION(#132)
SHAPE_REPRESENTATION_RELATIONSHIP()
);
#225=(
REPRESENTATION_RELATIONSHIP($,$,#17180,#17167)
REPRESENTATION_RELATIONSHIP_WITH_TRANSFORMATION(#133)
SHAPE_REPRESENTATION_RELATIONSHIP()
);
#226=(
REPRESENTATION_RELATIONSHIP($,$,#17181,#17167)
REPRESENTATION_RELATIONSHIP_WITH_TRANSFORMATION(#134)
SHAPE_REPRESENTATION_RELATIONSHIP()
);
#227=(
REPRESENTATION_RELATIONSHIP($,$,#17125,#17124)
REPRESENTATION_RELATIONSHIP_WITH_TRANSFORMATION(#135)
SHAPE_REPRESENTATION_RELATIONSHIP()
);
#228=(
REPRESENTATION_RELATIONSHIP($,$,#17143,#17124)
REPRESENTATION_RELATIONSHIP_WITH_TRANSFORMATION(#136)
SHAPE_REPRESENTATION_RELATIONSHIP()
);
#229=(
REPRESENTATION_RELATIONSHIP($,$,#17155,#17124)
REPRESENTATION_RELATIONSHIP_WITH_TRANSFORMATION(#137)
SHAPE_REPRESENTATION_RELATIONSHIP()
);
#230=(
REPRESENTATION_RELATIONSHIP($,$,#17167,#17124)
REPRESENTATION_RELATIONSHIP_WITH_TRANSFORMATION(#138)
SHAPE_REPRESENTATION_RELATIONSHIP()
);
#231=CONTEXT_DEPENDENT_SHAPE_REPRESENTATION(#139,#16989);
#232=CONTEXT_DEPENDENT_SHAPE_REPRESENTATION(#140,#16990);
#233=CONTEXT_DEPENDENT_SHAPE_REPRESENTATION(#141,#17019);
#234=CONTEXT_DEPENDENT_SHAPE_REPRESENTATION(#142,#17020);
#235=CONTEXT_DEPENDENT_SHAPE_REPRESENTATION(#143,#17021);
#236=CONTEXT_DEPENDENT_SHAPE_REPRESENTATION(#144,#17022);
#237=CONTEXT_DEPENDENT_SHAPE_REPRESENTATION(#145,#17023);
#238=CONTEXT_DEPENDENT_SHAPE_REPRESENTATION(#146,#17024);
#239=CONTEXT_DEPENDENT_SHAPE_REPRESENTATION(#147,#17025);
#240=CONTEXT_DEPENDENT_SHAPE_REPRESENTATION(#148,#17026);
#241=CONTEXT_DEPENDENT_SHAPE_REPRESENTATION(#149,#17027);
#242=CONTEXT_DEPENDENT_SHAPE_REPRESENTATION(#150,#17028);
#243=CONTEXT_DEPENDENT_SHAPE_REPRESENTATION(#151,#17029);
#244=CONTEXT_DEPENDENT_SHAPE_REPRESENTATION(#152,#17030);
#245=CONTEXT_DEPENDENT_SHAPE_REPRESENTATION(#153,#17042);
#246=CONTEXT_DEPENDENT_SHAPE_REPRESENTATION(#154,#17043);
#247=CONTEXT_DEPENDENT_SHAPE_REPRESENTATION(#155,#17044);
#248=CONTEXT_DEPENDENT_SHAPE_REPRESENTATION(#156,#17048);
#249=CONTEXT_DEPENDENT_SHAPE_REPRESENTATION(#157,#17049);
#250=CONTEXT_DEPENDENT_SHAPE_REPRESENTATION(#158,#17050);
#251=CONTEXT_DEPENDENT_SHAPE_REPRESENTATION(#159,#17051);
#252=CONTEXT_DEPENDENT_SHAPE_REPRESENTATION(#160,#17052);
#253=CONTEXT_DEPENDENT_SHAPE_REPRESENTATION(#161,#17053);
#254=CONTEXT_DEPENDENT_SHAPE_REPRESENTATION(#162,#17054);
#255=CONTEXT_DEPENDENT_SHAPE_REPRESENTATION(#163,#17055);
#256=CONTEXT_DEPENDENT_SHAPE_REPRESENTATION(#164,#17056);
#257=CONTEXT_DEPENDENT_SHAPE_REPRESENTATION(#165,#17057);
#258=CONTEXT_DEPENDENT_SHAPE_REPRESENTATION(#166,#17058);
#259=CONTEXT_DEPENDENT_SHAPE_REPRESENTATION(#167,#17059);
#260=CONTEXT_DEPENDENT_SHAPE_REPRESENTATION(#168,#17060);
#261=CONTEXT_DEPENDENT_SHAPE_REPRESENTATION(#169,#17061);
#262=CONTEXT_DEPENDENT_SHAPE_REPRESENTATION(#170,#17062);
#263=CONTEXT_DEPENDENT_SHAPE_REPRESENTATION(#171,#17063);
#264=CONTEXT_DEPENDENT_SHAPE_REPRESENTATION(#172,#17064);
#265=CONTEXT_DEPENDENT_SHAPE_REPRESENTATION(#173,#17065);
#266=CONTEXT_DEPENDENT_SHAPE_REPRESENTATION(#174,#17066);
#267=CONTEXT_DEPENDENT_SHAPE_REPRESENTATION(#175,#17067);
#268=CONTEXT_DEPENDENT_SHAPE_REPRESENTATION(#176,#17068);
#269=CONTEXT_DEPENDENT_SHAPE_REPRESENTATION(#177,#17069);
#270=CONTEXT_DEPENDENT_SHAPE_REPRESENTATION(#178,#17070);
#271=CONTEXT_DEPENDENT_SHAPE_REPRESENTATION(#179,#17071);
#272=CONTEXT_DEPENDENT_SHAPE_REPRESENTATION(#180,#17072);
#273=CONTEXT_DEPENDENT_SHAPE_REPRESENTATION(#181,#17073);
#274=CONTEXT_DEPENDENT_SHAPE_REPRESENTATION(#182,#17074);
#275=CONTEXT_DEPENDENT_SHAPE_REPRESENTATION(#183,#17075);
#276=CONTEXT_DEPENDENT_SHAPE_REPRESENTATION(#184,#17076);
#277=CONTEXT_DEPENDENT_SHAPE_REPRESENTATION(#185,#17077);
#278=CONTEXT_DEPENDENT_SHAPE_REPRESENTATION(#186,#17078);
#279=CONTEXT_DEPENDENT_SHAPE_REPRESENTATION(#187,#17079);
#280=CONTEXT_DEPENDENT_SHAPE_REPRESENTATION(#188,#17080);
#281=CONTEXT_DEPENDENT_SHAPE_REPRESENTATION(#189,#17081);
#282=CONTEXT_DEPENDENT_SHAPE_REPRESENTATION(#190,#17082);
#283=CONTEXT_DEPENDENT_SHAPE_REPRESENTATION(#191,#17083);
#284=CONTEXT_DEPENDENT_SHAPE_REPRESENTATION(#192,#17084);
#285=CONTEXT_DEPENDENT_SHAPE_REPRESENTATION(#193,#17086);
#286=CONTEXT_DEPENDENT_SHAPE_REPRESENTATION(#194,#17087);
#287=CONTEXT_DEPENDENT_SHAPE_REPRESENTATION(#195,#17088);
#288=CONTEXT_DEPENDENT_SHAPE_REPRESENTATION(#196,#17089);
#289=CONTEXT_DEPENDENT_SHAPE_REPRESENTATION(#197,#17090);
#290=CONTEXT_DEPENDENT_SHAPE_REPRESENTATION(#198,#17091);
#291=CONTEXT_DEPENDENT_SHAPE_REPRESENTATION(#199,#17092);
#292=CONTEXT_DEPENDENT_SHAPE_REPRESENTATION(#200,#17093);
#293=CONTEXT_DEPENDENT_SHAPE_REPRESENTATION(#201,#17094);
#294=CONTEXT_DEPENDENT_SHAPE_REPRESENTATION(#202,#17095);
#295=CONTEXT_DEPENDENT_SHAPE_REPRESENTATION(#203,#17096);
#296=CONTEXT_DEPENDENT_SHAPE_REPRESENTATION(#204,#17097);
#297=CONTEXT_DEPENDENT_SHAPE_REPRESENTATION(#205,#17098);
#298=CONTEXT_DEPENDENT_SHAPE_REPRESENTATION(#206,#17099);
#299=CONTEXT_DEPENDENT_SHAPE_REPRESENTATION(#207,#17100);
#300=CONTEXT_DEPENDENT_SHAPE_REPRESENTATION(#208,#17101);
#301=CONTEXT_DEPENDENT_SHAPE_REPRESENTATION(#209,#17102);
#302=CONTEXT_DEPENDENT_SHAPE_REPRESENTATION(#210,#17103);
#303=CONTEXT_DEPENDENT_SHAPE_REPRESENTATION(#211,#17104);
#304=CONTEXT_DEPENDENT_SHAPE_REPRESENTATION(#212,#17105);
#305=CONTEXT_DEPENDENT_SHAPE_REPRESENTATION(#213,#17106);
#306=CONTEXT_DEPENDENT_SHAPE_REPRESENTATION(#214,#17107);
#307=CONTEXT_DEPENDENT_SHAPE_REPRESENTATION(#215,#17108);
#308=CONTEXT_DEPENDENT_SHAPE_REPRESENTATION(#216,#17109);
#309=CONTEXT_DEPENDENT_SHAPE_REPRESENTATION(#217,#17110);
#310=CONTEXT_DEPENDENT_SHAPE_REPRESENTATION(#218,#17111);
#311=CONTEXT_DEPENDENT_SHAPE_REPRESENTATION(#219,#17112);
#312=CONTEXT_DEPENDENT_SHAPE_REPRESENTATION(#220,#17113);
#313=CONTEXT_DEPENDENT_SHAPE_REPRESENTATION(#221,#17114);
#314=CONTEXT_DEPENDENT_SHAPE_REPRESENTATION(#222,#17115);
#315=CONTEXT_DEPENDENT_SHAPE_REPRESENTATION(#223,#17116);
#316=CONTEXT_DEPENDENT_SHAPE_REPRESENTATION(#224,#17117);
#317=CONTEXT_DEPENDENT_SHAPE_REPRESENTATION(#225,#17118);
#318=CONTEXT_DEPENDENT_SHAPE_REPRESENTATION(#226,#17119);
#319=CONTEXT_DEPENDENT_SHAPE_REPRESENTATION(#227,#17120);
#320=CONTEXT_DEPENDENT_SHAPE_REPRESENTATION(#228,#17121);
#321=CONTEXT_DEPENDENT_SHAPE_REPRESENTATION(#229,#17122);
#322=CONTEXT_DEPENDENT_SHAPE_REPRESENTATION(#230,#17123);
#323=NEXT_ASSEMBLY_USAGE_OCCURRENCE('Housing:1','Housing:1','Housing:1',
#17195,#17196,'Housing:1');
#324=NEXT_ASSEMBLY_USAGE_OCCURRENCE('Insert bearing:1',
'Insert bearing:1','Insert bearing:1',#17195,#17197,'Insert bearing:1');
#325=NEXT_ASSEMBLY_USAGE_OCCURRENCE('Inner ring:1','Inner ring:1',
'Inner ring:1',#17220,#17221,'Inner ring:1');
#326=NEXT_ASSEMBLY_USAGE_OCCURRENCE('Outer ring:1','Outer ring:1',
'Outer ring:1',#17220,#17222,'Outer ring:1');
#327=NEXT_ASSEMBLY_USAGE_OCCURRENCE('Balls:1','Balls:1','Balls:1',#17220,
#17223,'Balls:1');
#328=NEXT_ASSEMBLY_USAGE_OCCURRENCE('Cage:1','Cage:1','Cage:1',#17220,#17224,
'Cage:1');
#329=NEXT_ASSEMBLY_USAGE_OCCURRENCE('Seals 2RS:1','Seals 2RS:1',
'Seals 2RS:1',#17220,#17225,'Seals 2RS:1');
#330=NEXT_ASSEMBLY_USAGE_OCCURRENCE('Connecting rod:1',
'Connecting rod:1','Connecting rod:1',#17214,#17215,'Connecting rod:1');
#331=NEXT_ASSEMBLY_USAGE_OCCURRENCE('Rod bearing retainer:1',
'Rod bearing retainer:1','Rod bearing retainer:1',#17214,#17216,
'Rod bearing retainer:1');
#332=NEXT_ASSEMBLY_USAGE_OCCURRENCE('Rod bearing retainer (1):1',
'Rod bearing retainer (1):1','Rod bearing retainer (1):1',#17214,#17217,
'Rod bearing retainer (1):1');
#333=NEXT_ASSEMBLY_USAGE_OCCURRENCE('Rod bearing retainer (2):1',
'Rod bearing retainer (2):1','Rod bearing retainer (2):1',#17214,#17218,
'Rod bearing retainer (2):1');
#334=NEXT_ASSEMBLY_USAGE_OCCURRENCE('Rod bearing retainer (3):1',
'Rod bearing retainer (3):1','Rod bearing retainer (3):1',#17214,#17219,
'Rod bearing retainer (3):1');
#335=NEXT_ASSEMBLY_USAGE_OCCURRENCE(
'Sealed Ball Bearing - 10 x 30 x 9 mm:2',
'Sealed Ball Bearing - 10 x 30 x 9 mm:2',
'Sealed Ball Bearing - 10 x 30 x 9 mm:2',#17214,#17220,
'Sealed Ball Bearing - 10 x 30 x 9 mm:2');
#336=NEXT_ASSEMBLY_USAGE_OCCURRENCE(
'Sealed Ball Bearing - 10 x 30 x 9 mm:3',
'Sealed Ball Bearing - 10 x 30 x 9 mm:3',
'Sealed Ball Bearing - 10 x 30 x 9 mm:3',#17214,#17220,
'Sealed Ball Bearing - 10 x 30 x 9 mm:3');
#337=NEXT_ASSEMBLY_USAGE_OCCURRENCE('Block:1','Block:1','Block:1',#17233,
#17234,'Block:1');
#338=NEXT_ASSEMBLY_USAGE_OCCURRENCE('End cap +:1','End cap +:1',
'End cap +:1',#17233,#17235,'End cap +:1');
#339=NEXT_ASSEMBLY_USAGE_OCCURRENCE('End cap:1','End cap:1','End cap:1',
#17233,#17236,'End cap:1');
#340=NEXT_ASSEMBLY_USAGE_OCCURRENCE('Base:1','Base:1','Base:1',#17184,#17185,
'Base:1');
#341=NEXT_ASSEMBLY_USAGE_OCCURRENCE('Bearing pedestal:1',
'Bearing pedestal:1','Bearing pedestal:1',#17184,#17186,
'Bearing pedestal:1');
#342=NEXT_ASSEMBLY_USAGE_OCCURRENCE('Bearing bolt reducer:1',
'Bearing bolt reducer:1','Bearing bolt reducer:1',#17184,#17187,
'Bearing bolt reducer:1');
#343=NEXT_ASSEMBLY_USAGE_OCCURRENCE('Bearing bolt reducer (1):1',
'Bearing bolt reducer (1):1','Bearing bolt reducer (1):1',#17184,#17188,
'Bearing bolt reducer (1):1');
#344=NEXT_ASSEMBLY_USAGE_OCCURRENCE('Bearing pedestal (1):1',
'Bearing pedestal (1):1','Bearing pedestal (1):1',#17184,#17189,
'Bearing pedestal (1):1');
#345=NEXT_ASSEMBLY_USAGE_OCCURRENCE('Bearing bolt reducer (2):1',
'Bearing bolt reducer (2):1','Bearing bolt reducer (2):1',#17184,#17190,
'Bearing bolt reducer (2):1');
#346=NEXT_ASSEMBLY_USAGE_OCCURRENCE('Bearing bolt reducer (3):1',
'Bearing bolt reducer (3):1','Bearing bolt reducer (3):1',#17184,#17191,
'Bearing bolt reducer (3):1');
#347=NEXT_ASSEMBLY_USAGE_OCCURRENCE('Rail pedestal:1','Rail pedestal:1',
'Rail pedestal:1',#17184,#17192,'Rail pedestal:1');
#348=NEXT_ASSEMBLY_USAGE_OCCURRENCE('Foot strip:1','Foot strip:1',
'Foot strip:1',#17184,#17193,'Foot strip:1');
#349=NEXT_ASSEMBLY_USAGE_OCCURRENCE('Foot strip (1):1',
'Foot strip (1):1','Foot strip (1):1',#17184,#17194,'Foot strip (1):1');
#350=NEXT_ASSEMBLY_USAGE_OCCURRENCE('Cap Screw - M5x20:2',
'Cap Screw - M5x20:2','Cap Screw - M5x20:2',#17184,#17239,
'Cap Screw - M5x20:2');
#351=NEXT_ASSEMBLY_USAGE_OCCURRENCE('Cap Screw - M5x20:3',
'Cap Screw - M5x20:3','Cap Screw - M5x20:3',#17184,#17239,
'Cap Screw - M5x20:3');
#352=NEXT_ASSEMBLY_USAGE_OCCURRENCE('Cap Screw - M5x20:4',
'Cap Screw - M5x20:4','Cap Screw - M5x20:4',#17184,#17239,
'Cap Screw - M5x20:4');
#353=NEXT_ASSEMBLY_USAGE_OCCURRENCE('Cap Screw - M5x20:5',
'Cap Screw - M5x20:5','Cap Screw - M5x20:5',#17184,#17239,
'Cap Screw - M5x20:5');
#354=NEXT_ASSEMBLY_USAGE_OCCURRENCE(
'Pillow Block Bearing - 20 mm Bore:2',
'Pillow Block Bearing - 20 mm Bore:2',
'Pillow Block Bearing - 20 mm Bore:2',#17184,#17195,
'Pillow Block Bearing - 20 mm Bore:2');
#355=NEXT_ASSEMBLY_USAGE_OCCURRENCE('Flat Washer - M8:2',
'Flat Washer - M8:2','Flat Washer - M8:2',#17184,#17198,
'Flat Washer - M8:2');
#356=NEXT_ASSEMBLY_USAGE_OCCURRENCE('M8x25 Bolt:2','M8x25 Bolt:2',
'M8x25 Bolt:2',#17184,#17199,'M8x25 Bolt:2');
#357=NEXT_ASSEMBLY_USAGE_OCCURRENCE('Flat Washer - M8:3',
'Flat Washer - M8:3','Flat Washer - M8:3',#17184,#17198,
'Flat Washer - M8:3');
#358=NEXT_ASSEMBLY_USAGE_OCCURRENCE('M8x25 Bolt:3','M8x25 Bolt:3',
'M8x25 Bolt:3',#17184,#17199,'M8x25 Bolt:3');
#359=NEXT_ASSEMBLY_USAGE_OCCURRENCE('Cap Screw - M5x20:6',
'Cap Screw - M5x20:6','Cap Screw - M5x20:6',#17184,#17239,
'Cap Screw - M5x20:6');
#360=NEXT_ASSEMBLY_USAGE_OCCURRENCE('Cap Screw - M5x20:7',
'Cap Screw - M5x20:7','Cap Screw - M5x20:7',#17184,#17239,
'Cap Screw - M5x20:7');
#361=NEXT_ASSEMBLY_USAGE_OCCURRENCE('Cap Screw - M5x20:8',
'Cap Screw - M5x20:8','Cap Screw - M5x20:8',#17184,#17239,
'Cap Screw - M5x20:8');
#362=NEXT_ASSEMBLY_USAGE_OCCURRENCE('Cap Screw - M5x20:9',
'Cap Screw - M5x20:9','Cap Screw - M5x20:9',#17184,#17239,
'Cap Screw - M5x20:9');
#363=NEXT_ASSEMBLY_USAGE_OCCURRENCE(
'Pillow Block Bearing - 20 mm Bore:3',
'Pillow Block Bearing - 20 mm Bore:3',
'Pillow Block Bearing - 20 mm Bore:3',#17184,#17195,
'Pillow Block Bearing - 20 mm Bore:3');
#364=NEXT_ASSEMBLY_USAGE_OCCURRENCE('Flat Washer - M8:4',
'Flat Washer - M8:4','Flat Washer - M8:4',#17184,#17198,
'Flat Washer - M8:4');
#365=NEXT_ASSEMBLY_USAGE_OCCURRENCE('M8x25 Bolt:4','M8x25 Bolt:4',
'M8x25 Bolt:4',#17184,#17199,'M8x25 Bolt:4');
#366=NEXT_ASSEMBLY_USAGE_OCCURRENCE('Flat Washer - M8:5',
'Flat Washer - M8:5','Flat Washer - M8:5',#17184,#17198,
'Flat Washer - M8:5');
#367=NEXT_ASSEMBLY_USAGE_OCCURRENCE('M8x25 Bolt:5','M8x25 Bolt:5',
'M8x25 Bolt:5',#17184,#17199,'M8x25 Bolt:5');
#368=NEXT_ASSEMBLY_USAGE_OCCURRENCE('M5x14 Cap Screw:2',
'M5x14 Cap Screw:2','M5x14 Cap Screw:2',#17184,#17237,
'M5x14 Cap Screw:2');
#369=NEXT_ASSEMBLY_USAGE_OCCURRENCE('M5x14 Cap Screw:3',
'M5x14 Cap Screw:3','M5x14 Cap Screw:3',#17184,#17237,
'M5x14 Cap Screw:3');
#370=NEXT_ASSEMBLY_USAGE_OCCURRENCE('M5x14 Cap Screw:4',
'M5x14 Cap Screw:4','M5x14 Cap Screw:4',#17184,#17237,
'M5x14 Cap Screw:4');
#371=NEXT_ASSEMBLY_USAGE_OCCURRENCE('M5x14 Cap Screw:5',
'M5x14 Cap Screw:5','M5x14 Cap Screw:5',#17184,#17237,
'M5x14 Cap Screw:5');
#372=NEXT_ASSEMBLY_USAGE_OCCURRENCE(
'Linear Guide Rail - 15 mm, 220 mm Long:2',
'Linear Guide Rail - 15 mm, 220 mm Long:2',
'Linear Guide Rail - 15 mm, 220 mm Long:2',#17184,#17200,
'Linear Guide Rail - 15 mm, 220 mm Long:2');
#373=NEXT_ASSEMBLY_USAGE_OCCURRENCE('Cap Screw - M4x16:2',
'Cap Screw - M4x16:2','Cap Screw - M4x16:2',#17184,#17201,
'Cap Screw - M4x16:2');
#374=NEXT_ASSEMBLY_USAGE_OCCURRENCE('Cap Screw - M4x16:3',
'Cap Screw - M4x16:3','Cap Screw - M4x16:3',#17184,#17201,
'Cap Screw - M4x16:3');
#375=NEXT_ASSEMBLY_USAGE_OCCURRENCE('Cap Screw - M4x16:4',
'Cap Screw - M4x16:4','Cap Screw - M4x16:4',#17184,#17201,
'Cap Screw - M4x16:4');
#376=NEXT_ASSEMBLY_USAGE_OCCURRENCE('Cap Screw - M4x16:5',
'Cap Screw - M4x16:5','Cap Screw - M4x16:5',#17184,#17201,
'Cap Screw - M4x16:5');
#377=NEXT_ASSEMBLY_USAGE_OCCURRENCE('Flywheel shaft:1',
'Flywheel shaft:1','Flywheel shaft:1',#17202,#17203,'Flywheel shaft:1');
#378=NEXT_ASSEMBLY_USAGE_OCCURRENCE('Shaft collar:1','Shaft collar:1',
'Shaft collar:1',#17202,#17204,'Shaft collar:1');
#379=NEXT_ASSEMBLY_USAGE_OCCURRENCE('Shaft collar (1):1',
'Shaft collar (1):1','Shaft collar (1):1',#17202,#17205,
'Shaft collar (1):1');
#380=NEXT_ASSEMBLY_USAGE_OCCURRENCE('Rear bearing spacer:1',
'Rear bearing spacer:1','Rear bearing spacer:1',#17202,#17206,
'Rear bearing spacer:1');
#381=NEXT_ASSEMBLY_USAGE_OCCURRENCE('Flywheel:1','Flywheel:1',
'Flywheel:1',#17202,#17207,'Flywheel:1');
#382=NEXT_ASSEMBLY_USAGE_OCCURRENCE('Crank pin:1','Crank pin:1',
'Crank pin:1',#17202,#17208,'Crank pin:1');
#383=NEXT_ASSEMBLY_USAGE_OCCURRENCE('Pin spacer 15 mm:1',
'Pin spacer 15 mm:1','Pin spacer 15 mm:1',#17202,#17209,
'Pin spacer 15 mm:1');
#384=NEXT_ASSEMBLY_USAGE_OCCURRENCE('Pin spacer 4 mm:1',
'Pin spacer 4 mm:1','Pin spacer 4 mm:1',#17202,#17210,
'Pin spacer 4 mm:1');
#385=NEXT_ASSEMBLY_USAGE_OCCURRENCE('Pin keeper:1','Pin keeper:1',
'Pin keeper:1',#17202,#17211,'Pin keeper:1');
#386=NEXT_ASSEMBLY_USAGE_OCCURRENCE('Key 6x6x20:2','Key 6x6x20:2',
'Key 6x6x20:2',#17202,#17212,'Key 6x6x20:2');
#387=NEXT_ASSEMBLY_USAGE_OCCURRENCE('Socket Set Screw - M5x8:2',
'Socket Set Screw - M5x8:2','Socket Set Screw - M5x8:2',#17202,#17213,
'Socket Set Screw - M5x8:2');
#388=NEXT_ASSEMBLY_USAGE_OCCURRENCE('Socket Set Screw - M5x8:3',
'Socket Set Screw - M5x8:3','Socket Set Screw - M5x8:3',#17202,#17213,
'Socket Set Screw - M5x8:3');
#389=NEXT_ASSEMBLY_USAGE_OCCURRENCE('Socket Set Screw - M5x8:4',
'Socket Set Screw - M5x8:4','Socket Set Screw - M5x8:4',#17202,#17213,
'Socket Set Screw - M5x8:4');
#390=NEXT_ASSEMBLY_USAGE_OCCURRENCE('M4x10 Cap Screw:2',
'M4x10 Cap Screw:2','M4x10 Cap Screw:2',#17202,#17240,
'M4x10 Cap Screw:2');
#391=NEXT_ASSEMBLY_USAGE_OCCURRENCE('Specimen carriage:1',
'Specimen carriage:1','Specimen carriage:1',#17226,#17227,
'Specimen carriage:1');
#392=NEXT_ASSEMBLY_USAGE_OCCURRENCE('Specimen clamp jaw:1',
'Specimen clamp jaw:1','Specimen clamp jaw:1',#17226,#17228,
'Specimen clamp jaw:1');
#393=NEXT_ASSEMBLY_USAGE_OCCURRENCE('Slider pin:1','Slider pin:1',
'Slider pin:1',#17226,#17229,'Slider pin:1');
#394=NEXT_ASSEMBLY_USAGE_OCCURRENCE('Pin spacer 2 mm:1',
'Pin spacer 2 mm:1','Pin spacer 2 mm:1',#17226,#17230,
'Pin spacer 2 mm:1');
#395=NEXT_ASSEMBLY_USAGE_OCCURRENCE('Pin spacer 4 mm (1):1',
'Pin spacer 4 mm (1):1','Pin spacer 4 mm (1):1',#17226,#17231,
'Pin spacer 4 mm (1):1');
#396=NEXT_ASSEMBLY_USAGE_OCCURRENCE('Pin keeper (1):1',
'Pin keeper (1):1','Pin keeper (1):1',#17226,#17232,'Pin keeper (1):1');
#397=NEXT_ASSEMBLY_USAGE_OCCURRENCE(
'Flanged Linear Guide Carriage - 15 mm:2',
'Flanged Linear Guide Carriage - 15 mm:2',
'Flanged Linear Guide Carriage - 15 mm:2',#17226,#17233,
'Flanged Linear Guide Carriage - 15 mm:2');
#398=NEXT_ASSEMBLY_USAGE_OCCURRENCE('Flat Washer - M5:2',
'Flat Washer - M5:2','Flat Washer - M5:2',#17226,#17238,
'Flat Washer - M5:2');
#399=NEXT_ASSEMBLY_USAGE_OCCURRENCE('M5x14 Cap Screw:6',
'M5x14 Cap Screw:6','M5x14 Cap Screw:6',#17226,#17237,
'M5x14 Cap Screw:6');
#400=NEXT_ASSEMBLY_USAGE_OCCURRENCE('Flat Washer - M5:3',
'Flat Washer - M5:3','Flat Washer - M5:3',#17226,#17238,
'Flat Washer - M5:3');
#401=NEXT_ASSEMBLY_USAGE_OCCURRENCE('M5x14 Cap Screw:7',
'M5x14 Cap Screw:7','M5x14 Cap Screw:7',#17226,#17237,
'M5x14 Cap Screw:7');
#402=NEXT_ASSEMBLY_USAGE_OCCURRENCE('Flat Washer - M5:4',
'Flat Washer - M5:4','Flat Washer - M5:4',#17226,#17238,
'Flat Washer - M5:4');
#403=NEXT_ASSEMBLY_USAGE_OCCURRENCE('M5x14 Cap Screw:8',
'M5x14 Cap Screw:8','M5x14 Cap Screw:8',#17226,#17237,
'M5x14 Cap Screw:8');
#404=NEXT_ASSEMBLY_USAGE_OCCURRENCE('Flat Washer - M5:5',
'Flat Washer - M5:5','Flat Washer - M5:5',#17226,#17238,
'Flat Washer - M5:5');
#405=NEXT_ASSEMBLY_USAGE_OCCURRENCE('M5x14 Cap Screw:9',
'M5x14 Cap Screw:9','M5x14 Cap Screw:9',#17226,#17237,
'M5x14 Cap Screw:9');
#406=NEXT_ASSEMBLY_USAGE_OCCURRENCE('Flat Washer - M5:6',
'Flat Washer - M5:6','Flat Washer - M5:6',#17226,#17238,
'Flat Washer - M5:6');
#407=NEXT_ASSEMBLY_USAGE_OCCURRENCE('Cap Screw - M5x20:10',
'Cap Screw - M5x20:10','Cap Screw - M5x20:10',#17226,#17239,
'Cap Screw - M5x20:10');
#408=NEXT_ASSEMBLY_USAGE_OCCURRENCE('Flat Washer - M5:7',
'Flat Washer - M5:7','Flat Washer - M5:7',#17226,#17238,
'Flat Washer - M5:7');
#409=NEXT_ASSEMBLY_USAGE_OCCURRENCE('Cap Screw - M5x20:11',
'Cap Screw - M5x20:11','Cap Screw - M5x20:11',#17226,#17239,
'Cap Screw - M5x20:11');
#410=NEXT_ASSEMBLY_USAGE_OCCURRENCE('M4x10 Cap Screw:3',
'M4x10 Cap Screw:3','M4x10 Cap Screw:3',#17226,#17240,
'M4x10 Cap Screw:3');
#411=NEXT_ASSEMBLY_USAGE_OCCURRENCE('Bearing and guide frame:1',
'Bearing and guide frame:1','Bearing and guide frame:1',#17183,#17184,
'Bearing and guide frame:1');
#412=NEXT_ASSEMBLY_USAGE_OCCURRENCE('Flywheel and crank:1',
'Flywheel and crank:1','Flywheel and crank:1',#17183,#17202,
'Flywheel and crank:1');
#413=NEXT_ASSEMBLY_USAGE_OCCURRENCE('Connecting rod (1):1',
'Connecting rod (1):1','Connecting rod (1):1',#17183,#17214,
'Connecting rod (1):1');
#414=NEXT_ASSEMBLY_USAGE_OCCURRENCE('Guided slider:1','Guided slider:1',
'Guided slider:1',#17183,#17226,'Guided slider:1');
#415=B_SPLINE_CURVE_WITH_KNOTS('',3,(#14016,#14017,#14018,#14019,#14020,
#14021,#14022,#14023,#14024,#14025),.UNSPECIFIED.,.F.,.F.,(4,2,2,2,4),(1.13193471301885,
1.22626174930539,1.32058878559194,1.41491753480854,1.50924628402513),
 .UNSPECIFIED.);
#416=B_SPLINE_CURVE_WITH_KNOTS('',3,(#14027,#14028,#14029,#14030,#14031,
#14032,#14033,#14034,#14035,#14036,#14037,#14038,#14039,#14040,#14041,#14042,
#14043,#14044),.UNSPECIFIED.,.F.,.F.,(4,2,2,2,2,2,2,2,4),(0.377311571006283,
0.471638607292829,0.565965643579376,0.66029439279597,0.754623142012565,
0.84895189122916,0.943280640445754,1.0376076767323,1.13193471301885),
 .UNSPECIFIED.);
#417=B_SPLINE_CURVE_WITH_KNOTS('',3,(#14045,#14046,#14047,#14048,#14049,
#14050,#14051,#14052,#14053,#14054),.UNSPECIFIED.,.F.,.F.,(4,2,2,2,4),(1.50924628402513,
1.60357503324173,1.69790378245832,1.79223081874487,1.88655785503141),
 .UNSPECIFIED.);
#418=B_SPLINE_CURVE_WITH_KNOTS('',3,(#14057,#14058,#14059,#14060,#14061,
#14062,#14063,#14064,#14065,#14066,#14067,#14068,#14069,#14070,#14071,#14072,
#14073,#14074,#14075,#14076,#14077,#14078,#14079,#14080,#14081,#14082,#14083,
#14084,#14085,#14086,#14087,#14088,#14089,#14090),.UNSPECIFIED.,.T.,.F.,
(4,2,2,2,2,2,2,2,2,2,2,2,2,2,2,2,4),(0.,0.0946120580087934,0.189224116017587,
0.283822945575014,0.378421775132442,0.47302060468987,0.567619434247297,
0.662231492256091,0.756843550264884,0.851455608273677,0.94606766628247,
1.0406664958399,1.13526532539733,1.22986415495475,1.32446298451218,1.41907504252097,
1.51368710052977),.UNSPECIFIED.);
#419=B_SPLINE_CURVE_WITH_KNOTS('',3,(#14093,#14094,#14095,#14096,#14097,
#14098,#14099,#14100,#14101,#14102,#14103,#14104,#14105,#14106,#14107,#14108,
#14109,#14110,#14111,#14112,#14113,#14114,#14115,#14116,#14117,#14118,#14119,
#14120,#14121,#14122,#14123,#14124,#14125,#14126),.UNSPECIFIED.,.T.,.F.,
(4,2,2,2,2,2,2,2,2,2,2,2,2,2,2,2,4),(0.,0.0946120580087934,0.189224116017587,
0.283822945575014,0.378421775132442,0.47302060468987,0.567619434247297,
0.66223149225609,0.756843550264884,0.851455608273677,0.94606766628247,1.0406664958399,
1.13526532539733,1.22986415495475,1.32446298451218,1.41907504252097,1.51368710052977),
 .UNSPECIFIED.);
#420=B_SPLINE_CURVE_WITH_KNOTS('',3,(#14130,#14131,#14132,#14133,#14134,
#14135,#14136,#14137,#14138,#14139),.UNSPECIFIED.,.F.,.F.,(4,2,2,2,4),(1.13193471301885,
1.22626174930539,1.32058878559194,1.41491753480854,1.50924628402513),
 .UNSPECIFIED.);
#421=B_SPLINE_CURVE_WITH_KNOTS('',3,(#14141,#14142,#14143,#14144,#14145,
#14146,#14147,#14148,#14149,#14150,#14151,#14152,#14153,#14154,#14155,#14156,
#14157,#14158),.UNSPECIFIED.,.F.,.F.,(4,2,2,2,2,2,2,2,4),(0.377311571006283,
0.47163860729283,0.565965643579376,0.660294392795971,0.754623142012565,
0.84895189122916,0.943280640445755,1.0376076767323,1.13193471301885),
 .UNSPECIFIED.);
#422=B_SPLINE_CURVE_WITH_KNOTS('',3,(#14159,#14160,#14161,#14162,#14163,
#14164,#14165,#14166,#14167,#14168),.UNSPECIFIED.,.F.,.F.,(4,2,2,2,4),(1.50924628402513,
1.60357503324173,1.69790378245832,1.79223081874487,1.88655785503141),
 .UNSPECIFIED.);
#423=B_SPLINE_CURVE_WITH_KNOTS('',3,(#14177,#14178,#14179,#14180,#14181,
#14182,#14183,#14184,#14185,#14186,#14187,#14188,#14189,#14190,#14191,#14192,
#14193,#14194),.UNSPECIFIED.,.F.,.F.,(4,2,2,2,2,2,2,2,4),(0.377311571006282,
0.471638607292829,0.565965643579376,0.660294392795971,0.754623142012565,
0.84895189122916,0.943280640445754,1.0376076767323,1.13193471301885),
 .UNSPECIFIED.);
#424=B_SPLINE_CURVE_WITH_KNOTS('',3,(#14196,#14197,#14198,#14199,#14200,
#14201,#14202,#14203,#14204,#14205),.UNSPECIFIED.,.F.,.F.,(4,2,2,2,4),(1.13193471301885,
1.22626174930539,1.32058878559194,1.41491753480854,1.50924628402513),
 .UNSPECIFIED.);
#425=B_SPLINE_CURVE_WITH_KNOTS('',3,(#14206,#14207,#14208,#14209,#14210,
#14211,#14212,#14213,#14214,#14215),.UNSPECIFIED.,.F.,.F.,(4,2,2,2,4),(1.50924628402513,
1.60357503324172,1.69790378245832,1.79223081874487,1.88655785503141),
 .UNSPECIFIED.);
#426=B_SPLINE_CURVE_WITH_KNOTS('',3,(#14218,#14219,#14220,#14221,#14222,
#14223,#14224,#14225,#14226,#14227,#14228,#14229,#14230,#14231,#14232,#14233,
#14234,#14235),.UNSPECIFIED.,.F.,.F.,(4,2,2,2,2,2,2,2,4),(0.377311571006283,
0.47163860729283,0.565965643579376,0.660294392795971,0.754623142012565,
0.84895189122916,0.943280640445754,1.0376076767323,1.13193471301885),
 .UNSPECIFIED.);
#427=B_SPLINE_CURVE_WITH_KNOTS('',3,(#14237,#14238,#14239,#14240,#14241,
#14242,#14243,#14244,#14245,#14246),.UNSPECIFIED.,.F.,.F.,(4,2,2,2,4),(1.13193471301885,
1.22626174930539,1.32058878559194,1.41491753480854,1.50924628402513),
 .UNSPECIFIED.);
#428=B_SPLINE_CURVE_WITH_KNOTS('',3,(#14247,#14248,#14249,#14250,#14251,
#14252,#14253,#14254,#14255,#14256),.UNSPECIFIED.,.F.,.F.,(4,2,2,2,4),(1.50924628402513,
1.60357503324173,1.69790378245832,1.79223081874487,1.88655785503141),
 .UNSPECIFIED.);
#429=B_SPLINE_CURVE_WITH_KNOTS('',3,(#14259,#14260,#14261,#14262,#14263,
#14264,#14265,#14266,#14267,#14268,#14269,#14270,#14271,#14272,#14273,#14274,
#14275,#14276),.UNSPECIFIED.,.F.,.F.,(4,2,2,2,2,2,2,2,4),(0.377311571006282,
0.471638607292829,0.565965643579376,0.66029439279597,0.754623142012565,
0.84895189122916,0.943280640445754,1.0376076767323,1.13193471301885),
 .UNSPECIFIED.);
#430=B_SPLINE_CURVE_WITH_KNOTS('',3,(#14278,#14279,#14280,#14281,#14282,
#14283,#14284,#14285,#14286,#14287),.UNSPECIFIED.,.F.,.F.,(4,2,2,2,4),(1.13193471301885,
1.22626174930539,1.32058878559194,1.41491753480854,1.50924628402513),
 .UNSPECIFIED.);
#431=B_SPLINE_CURVE_WITH_KNOTS('',3,(#14288,#14289,#14290,#14291,#14292,
#14293,#14294,#14295,#14296,#14297),.UNSPECIFIED.,.F.,.F.,(4,2,2,2,4),(1.50924628402513,
1.60357503324172,1.69790378245832,1.79223081874487,1.88655785503141),
 .UNSPECIFIED.);
#432=B_SPLINE_CURVE_WITH_KNOTS('',3,(#14300,#14301,#14302,#14303,#14304,
#14305,#14306,#14307,#14308,#14309,#14310,#14311,#14312,#14313,#14314,#14315,
#14316,#14317),.UNSPECIFIED.,.F.,.F.,(4,2,2,2,2,2,2,2,4),(0.377311571006283,
0.471638607292829,0.565965643579376,0.660294392795971,0.754623142012565,
0.84895189122916,0.943280640445755,1.0376076767323,1.13193471301885),
 .UNSPECIFIED.);
#433=B_SPLINE_CURVE_WITH_KNOTS('',3,(#14319,#14320,#14321,#14322,#14323,
#14324,#14325,#14326,#14327,#14328),.UNSPECIFIED.,.F.,.F.,(4,2,2,2,4),(1.13193471301885,
1.22626174930539,1.32058878559194,1.41491753480854,1.50924628402513),
 .UNSPECIFIED.);
#434=B_SPLINE_CURVE_WITH_KNOTS('',3,(#14329,#14330,#14331,#14332,#14333,
#14334,#14335,#14336,#14337,#14338),.UNSPECIFIED.,.F.,.F.,(4,2,2,2,4),(1.50924628402513,
1.60357503324172,1.69790378245832,1.79223081874487,1.88655785503141),
 .UNSPECIFIED.);
#435=B_SPLINE_CURVE_WITH_KNOTS('',3,(#14342,#14343,#14344,#14345,#14346,
#14347,#14348,#14349,#14350,#14351,#14352,#14353,#14354,#14355,#14356,#14357,
#14358,#14359,#14360,#14361,#14362,#14363,#14364,#14365,#14366,#14367,#14368,
#14369,#14370,#14371,#14372,#14373,#14374,#14375),.UNSPECIFIED.,.T.,.F.,
(4,2,2,2,2,2,2,2,2,2,2,2,2,2,2,2,4),(0.,0.0946120580087934,0.189224116017587,
0.283822945575014,0.378421775132442,0.47302060468987,0.567619434247297,
0.66223149225609,0.756843550264884,0.851455608273677,0.94606766628247,1.0406664958399,
1.13526532539733,1.22986415495475,1.32446298451218,1.41907504252097,1.51368710052977),
 .UNSPECIFIED.);
#436=B_SPLINE_CURVE_WITH_KNOTS('',3,(#14378,#14379,#14380,#14381,#14382,
#14383,#14384,#14385,#14386,#14387,#14388,#14389,#14390,#14391,#14392,#14393,
#14394,#14395,#14396,#14397,#14398,#14399,#14400,#14401,#14402,#14403,#14404,
#14405,#14406,#14407,#14408,#14409,#14410,#14411),.UNSPECIFIED.,.T.,.F.,
(4,2,2,2,2,2,2,2,2,2,2,2,2,2,2,2,4),(0.,0.0946120580087934,0.189224116017587,
0.283822945575014,0.378421775132442,0.47302060468987,0.567619434247297,
0.66223149225609,0.756843550264884,0.851455608273677,0.94606766628247,1.0406664958399,
1.13526532539733,1.22986415495475,1.32446298451218,1.41907504252097,1.51368710052977),
 .UNSPECIFIED.);
#437=B_SPLINE_CURVE_WITH_KNOTS('',3,(#14416,#14417,#14418,#14419,#14420,
#14421,#14422,#14423,#14424,#14425,#14426,#14427,#14428,#14429,#14430,#14431,
#14432,#14433,#14434,#14435,#14436,#14437,#14438,#14439,#14440,#14441,#14442,
#14443,#14444,#14445,#14446,#14447,#14448,#14449),.UNSPECIFIED.,.T.,.F.,
(4,2,2,2,2,2,2,2,2,2,2,2,2,2,2,2,4),(0.,0.0946120580087934,0.189224116017587,
0.283822945575014,0.378421775132442,0.47302060468987,0.567619434247297,
0.66223149225609,0.756843550264884,0.851455608273677,0.94606766628247,1.0406664958399,
1.13526532539733,1.22986415495475,1.32446298451218,1.41907504252097,1.51368710052977),
 .UNSPECIFIED.);
#438=B_SPLINE_CURVE_WITH_KNOTS('',3,(#14452,#14453,#14454,#14455,#14456,
#14457,#14458,#14459,#14460,#14461,#14462,#14463,#14464,#14465,#14466,#14467,
#14468,#14469,#14470,#14471,#14472,#14473,#14474,#14475,#14476,#14477,#14478,
#14479,#14480,#14481,#14482,#14483,#14484,#14485),.UNSPECIFIED.,.T.,.F.,
(4,2,2,2,2,2,2,2,2,2,2,2,2,2,2,2,4),(0.,0.0946120580087934,0.189224116017587,
0.283822945575014,0.378421775132442,0.47302060468987,0.567619434247297,
0.66223149225609,0.756843550264884,0.851455608273677,0.94606766628247,1.0406664958399,
1.13526532539733,1.22986415495475,1.32446298451218,1.41907504252097,1.51368710052977),
 .UNSPECIFIED.);
#439=B_SPLINE_CURVE_WITH_KNOTS('',3,(#14824,#14825,#14826,#14827,#14828,
#14829,#14830,#14831,#14832,#14833,#14834,#14835,#14836,#14837),
 .UNSPECIFIED.,.F.,.F.,(4,2,2,2,2,2,4),(0.756005737987026,0.793568827564645,
0.8729225200542,0.952276212543755,1.03162990503331,1.11098359752287,1.14854668710048),
 .UNSPECIFIED.);
#440=B_SPLINE_CURVE_WITH_KNOTS('',3,(#14843,#14844,#14845,#14846,#14847,
#14848,#14849,#14850,#14851,#14852,#14853,#14854,#14855,#14856,#14857,#14858,
#14859,#14860),.UNSPECIFIED.,.F.,.F.,(4,2,2,2,2,2,2,2,4),(0.,0.0792165807733624,
0.158433161546725,0.23764869707457,0.316864232602414,0.396079768130259,
0.475295303658103,0.554511884431466,0.633728465204828),.UNSPECIFIED.);
#441=B_SPLINE_CURVE_WITH_KNOTS('',3,(#14861,#14862,#14863,#14864,#14865,
#14866,#14867,#14868,#14869,#14870,#14871,#14872,#14873,#14874,#14875,#14876,
#14877,#14878),.UNSPECIFIED.,.F.,.F.,(4,2,2,2,2,2,2,2,4),(0.633728465204828,
0.712945045978191,0.792161626751553,0.871377162279398,0.950592697807242,
1.02980823333509,1.10902376886293,1.18824034963629,1.26745693040966),
 .UNSPECIFIED.);
#442=B_SPLINE_CURVE_WITH_KNOTS('',3,(#14881,#14882,#14883,#14884,#14885,
#14886,#14887,#14888,#14889,#14890,#14891,#14892,#14893,#14894),
 .UNSPECIFIED.,.F.,.F.,(4,2,2,2,2,2,4),(0.121154929624525,0.158718019202141,
0.238071711691697,0.317425404181252,0.396779096670807,0.476132789160362,
0.513695878737981),.UNSPECIFIED.);
#443=B_SPLINE_CURVE_WITH_KNOTS('',3,(#14919,#14920,#14921,#14922,#14923,
#14924,#14925,#14926,#14927,#14928,#14929,#14930,#14931,#14932),
 .UNSPECIFIED.,.F.,.F.,(4,2,2,2,2,2,4),(0.756005737987028,0.793568827564648,
0.872922520054202,0.952276212543757,1.03162990503331,1.11098359752287,1.14854668710049),
 .UNSPECIFIED.);
#444=B_SPLINE_CURVE_WITH_KNOTS('',3,(#14938,#14939,#14940,#14941,#14942,
#14943,#14944,#14945,#14946,#14947,#14948,#14949,#14950,#14951,#14952,#14953,
#14954,#14955),.UNSPECIFIED.,.F.,.F.,(4,2,2,2,2,2,2,2,4),(0.,0.0792165807733633,
0.158433161546727,0.237648697074571,0.316864232602415,0.396079768130259,
0.475295303658103,0.554511884431466,0.63372846520483),.UNSPECIFIED.);
#445=B_SPLINE_CURVE_WITH_KNOTS('',3,(#14956,#14957,#14958,#14959,#14960,
#14961,#14962,#14963,#14964,#14965,#14966,#14967,#14968,#14969,#14970,#14971,
#14972,#14973),.UNSPECIFIED.,.F.,.F.,(4,2,2,2,2,2,2,2,4),(0.63372846520483,
0.712945045978193,0.792161626751556,0.8713771622794,0.950592697807245,1.02980823333509,
1.10902376886293,1.1882403496363,1.26745693040966),.UNSPECIFIED.);
#446=B_SPLINE_CURVE_WITH_KNOTS('',3,(#14976,#14977,#14978,#14979,#14980,
#14981,#14982,#14983,#14984,#14985,#14986,#14987,#14988,#14989),
 .UNSPECIFIED.,.F.,.F.,(4,2,2,2,2,2,4),(0.121154929624524,0.158718019202143,
0.238071711691698,0.317425404181252,0.396779096670807,0.476132789160362,
0.513695878737981),.UNSPECIFIED.);
#447=B_SPLINE_CURVE_WITH_KNOTS('',3,(#15046,#15047,#15048,#15049,#15050,
#15051),.UNSPECIFIED.,.F.,.F.,(4,2,4),(1.01510699658258,1.03166343394832,
1.10079263710785),.UNSPECIFIED.);
#448=B_SPLINE_CURVE_WITH_KNOTS('',3,(#15055,#15056,#15057,#15058,#15059,
#15060,#15061,#15062,#15063,#15064),.UNSPECIFIED.,.F.,.F.,(4,2,2,2,4),(0.168950313426779,
0.238079516586307,0.317435737633656,0.396791958681006,0.465921161840534),
 .UNSPECIFIED.);
#449=B_SPLINE_CURVE_WITH_KNOTS('',3,(#15068,#15069,#15070,#15071,#15072,
#15073),.UNSPECIFIED.,.F.,.F.,(4,2,4),(0.803821788694091,0.872950991853619,
0.88950742921936),.UNSPECIFIED.);
#450=B_SPLINE_CURVE_WITH_KNOTS('',3,(#15103,#15104,#15105,#15106,#15107,
#15108,#15109,#15110,#15111,#15112,#15113,#15114,#15115,#15116,#15117,#15118,
#15119,#15120,#15121,#15122,#15123,#15124,#15125,#15126,#15127,#15128,#15129,
#15130,#15131,#15132,#15133,#15134,#15135,#15136,#15137),.UNSPECIFIED.,
 .F.,.F.,(4,2,2,2,2,2,2,2,2,2,2,2,3,2,2,2,4),(0.379554434981269,0.396011596624156,
0.475213593758045,0.554416396369289,0.633619198980533,0.712822001591777,
0.792024804203021,0.87122680133691,0.950428798470799,1.02963079560469,1.10883279273858,
1.18803559534982,1.26723839796107,1.34644120057231,1.42564400318355,1.50484600031744,
1.52130316196033),.UNSPECIFIED.);
#451=B_SPLINE_CURVE_WITH_KNOTS('',3,(#15536,#15537,#15538,#15539,#15540,
#15541,#15542,#15543,#15544,#15545,#15546,#15547,#15548,#15549,#15550,#15551,
#15552,#15553,#15554,#15555,#15556,#15557),.UNSPECIFIED.,.F.,.F.,(4,2,2,
2,2,2,2,2,2,2,4),(0.0473477652366656,0.126350602536658,0.189525903804987,
0.252701205073317,0.313298422430275,0.373895639787233,0.434492857144191,
0.495090074501149,0.558265375769478,0.621440677037807,0.7004435143378),
 .UNSPECIFIED.);
#452=B_SPLINE_CURVE_WITH_KNOTS('',3,(#15561,#15562,#15563,#15564,#15565,
#15566,#15567,#15568,#15569,#15570,#15571,#15572,#15573,#15574,#15575,#15576,
#15577,#15578,#15579,#15580,#15581,#15582),.UNSPECIFIED.,.F.,.F.,(4,2,2,
2,2,2,2,2,2,2,4),(0.0464897534940957,0.0852567806515119,0.170513561303024,
0.246687263103517,0.308657850341199,0.370628437578881,0.432599024816563,
0.494569612054245,0.570743313854739,0.656000094506251,0.694767121663666),
 .UNSPECIFIED.);
#453=B_SPLINE_CURVE_WITH_KNOTS('',3,(#15588,#15589,#15590,#15591,#15592,
#15593,#15594,#15595,#15596,#15597,#15598,#15599,#15600,#15601,#15602,#15603,
#15604,#15605,#15606,#15607,#15608,#15609),.UNSPECIFIED.,.F.,.F.,(4,2,2,
2,2,2,2,2,2,2,4),(0.0464897534940957,0.0852567806515118,0.170513561303024,
0.246687263103517,0.308657850341199,0.370628437578881,0.432599024816563,
0.494569612054245,0.570743313854738,0.65600009450625,0.694767121663666),
 .UNSPECIFIED.);
#454=B_SPLINE_CURVE_WITH_KNOTS('',3,(#15613,#15614,#15615,#15616,#15617,
#15618,#15619,#15620,#15621,#15622,#15623,#15624,#15625,#15626,#15627,#15628,
#15629,#15630,#15631,#15632,#15633,#15634),.UNSPECIFIED.,.F.,.F.,(4,2,2,
2,2,2,2,2,2,2,4),(0.0464897534940957,0.0852567806515119,0.170513561303024,
0.246687263103517,0.308657850341199,0.370628437578881,0.432599024816563,
0.494569612054245,0.570743313854739,0.656000094506251,0.694767121663666),
 .UNSPECIFIED.);
#455=B_SPLINE_CURVE_WITH_KNOTS('',3,(#15638,#15639,#15640,#15641,#15642,
#15643,#15644,#15645,#15646,#15647,#15648,#15649),.UNSPECIFIED.,.F.,.F.,
(4,2,2,2,2,4),(0.0464897534940957,0.0852567806515119,0.170513561303024,
0.246687263103517,0.308657850341199,0.370628437578881),.UNSPECIFIED.);
#456=B_SPLINE_CURVE_WITH_KNOTS('',3,(#15654,#15655,#15656,#15657,#15658,
#15659,#15660,#15661,#15662,#15663,#15664,#15665),.UNSPECIFIED.,.F.,.F.,
(4,2,2,2,2,4),(0.370628437578881,0.432599024816563,0.494569612054245,0.570743313854738,
0.65600009450625,0.694767121663666),.UNSPECIFIED.);
#457=B_SPLINE_CURVE_WITH_KNOTS('',3,(#15669,#15670,#15671,#15672,#15673,
#15674,#15675,#15676,#15677,#15678,#15679,#15680,#15681,#15682,#15683,#15684,
#15685,#15686,#15687,#15688,#15689,#15690),.UNSPECIFIED.,.F.,.F.,(4,2,2,
2,2,2,2,2,2,2,4),(0.0464897534940957,0.0852567806515121,0.170513561303024,
0.246687263103518,0.308657850341199,0.370628437578881,0.432599024816563,
0.494569612054245,0.570743313854738,0.65600009450625,0.694767121663666),
 .UNSPECIFIED.);
#458=B_SPLINE_CURVE_WITH_KNOTS('',3,(#15694,#15695,#15696,#15697,#15698,
#15699,#15700,#15701,#15702,#15703,#15704,#15705,#15706,#15707,#15708,#15709,
#15710,#15711,#15712,#15713,#15714,#15715),.UNSPECIFIED.,.F.,.F.,(4,2,2,
2,2,2,2,2,2,2,4),(0.0464897534940957,0.0852567806515119,0.170513561303024,
0.246687263103517,0.308657850341199,0.370628437578881,0.432599024816563,
0.494569612054245,0.570743313854738,0.65600009450625,0.694767121663667),
 .UNSPECIFIED.);
#459=B_SPLINE_CURVE_WITH_KNOTS('',3,(#15719,#15720,#15721,#15722,#15723,
#15724,#15725,#15726,#15727,#15728,#15729,#15730,#15731,#15732,#15733,#15734,
#15735,#15736,#15737,#15738,#15739,#15740),.UNSPECIFIED.,.F.,.F.,(4,2,2,
2,2,2,2,2,2,2,4),(0.0464897534940957,0.0852567806515119,0.170513561303024,
0.246687263103517,0.308657850341199,0.370628437578881,0.432599024816563,
0.494569612054245,0.570743313854738,0.65600009450625,0.694767121663666),
 .UNSPECIFIED.);
#460=B_SPLINE_CURVE_WITH_KNOTS('',3,(#15744,#15745,#15746,#15747,#15748,
#15749,#15750,#15751,#15752,#15753,#15754,#15755,#15756,#15757,#15758,#15759,
#15760,#15761,#15762,#15763,#15764,#15765),.UNSPECIFIED.,.F.,.F.,(4,2,2,
2,2,2,2,2,2,2,4),(0.0464897534940957,0.0852567806515119,0.170513561303024,
0.246687263103517,0.308657850341199,0.370628437578881,0.432599024816563,
0.494569612054245,0.570743313854739,0.656000094506251,0.694767121663667),
 .UNSPECIFIED.);
#461=B_SPLINE_CURVE_WITH_KNOTS('',3,(#15773,#15774,#15775,#15776,#15777,
#15778,#15779,#15780,#15781,#15782,#15783,#15784,#15785,#15786,#15787,#15788,
#15789,#15790,#15791,#15792,#15793,#15794),.UNSPECIFIED.,.F.,.F.,(4,2,2,
2,2,2,2,2,2,2,4),(0.0473477652366656,0.126350602536658,0.189525903804987,
0.252701205073316,0.313298422430274,0.373895639787232,0.434492857144191,
0.495090074501149,0.558265375769478,0.621440677037807,0.7004435143378),
 .UNSPECIFIED.);
#462=B_SPLINE_CURVE_WITH_KNOTS('',3,(#15802,#15803,#15804,#15805,#15806,
#15807,#15808,#15809,#15810,#15811,#15812,#15813,#15814,#15815,#15816,#15817,
#15818,#15819,#15820,#15821,#15822,#15823),.UNSPECIFIED.,.F.,.F.,(4,2,2,
2,2,2,2,2,2,2,4),(0.0473477652366656,0.126350602536658,0.189525903804987,
0.252701205073317,0.313298422430275,0.373895639787233,0.434492857144191,
0.495090074501149,0.558265375769478,0.621440677037807,0.7004435143378),
 .UNSPECIFIED.);
#463=B_SPLINE_CURVE_WITH_KNOTS('',3,(#15832,#15833,#15834,#15835,#15836,
#15837,#15838,#15839,#15840,#15841,#15842,#15843),.UNSPECIFIED.,.F.,.F.,
(4,2,2,2,2,4),(0.0473477652366656,0.126350602536658,0.189525903804987,0.252701205073316,
0.313298422430275,0.373895639787233),.UNSPECIFIED.);
#464=B_SPLINE_CURVE_WITH_KNOTS('',3,(#15845,#15846,#15847,#15848,#15849,
#15850,#15851,#15852,#15853,#15854,#15855,#15856),.UNSPECIFIED.,.F.,.F.,
(4,2,2,2,2,4),(0.373895639787233,0.434492857144191,0.495090074501149,0.558265375769478,
0.621440677037807,0.7004435143378),.UNSPECIFIED.);
#465=B_SPLINE_CURVE_WITH_KNOTS('',3,(#15863,#15864,#15865,#15866,#15867,
#15868,#15869,#15870,#15871,#15872,#15873,#15874,#15875,#15876,#15877,#15878,
#15879,#15880,#15881,#15882,#15883,#15884),.UNSPECIFIED.,.F.,.F.,(4,2,2,
2,2,2,2,2,2,2,4),(0.0473477652366656,0.126350602536658,0.189525903804987,
0.252701205073316,0.313298422430275,0.373895639787233,0.434492857144191,
0.495090074501149,0.558265375769478,0.621440677037807,0.7004435143378),
 .UNSPECIFIED.);
#466=B_SPLINE_CURVE_WITH_KNOTS('',3,(#15892,#15893,#15894,#15895,#15896,
#15897,#15898,#15899,#15900,#15901,#15902,#15903,#15904,#15905,#15906,#15907,
#15908,#15909,#15910,#15911,#15912,#15913),.UNSPECIFIED.,.F.,.F.,(4,2,2,
2,2,2,2,2,2,2,4),(0.0473477652366656,0.126350602536658,0.189525903804987,
0.252701205073317,0.313298422430275,0.373895639787233,0.434492857144191,
0.495090074501149,0.558265375769478,0.621440677037807,0.7004435143378),
 .UNSPECIFIED.);
#467=B_SPLINE_CURVE_WITH_KNOTS('',3,(#15921,#15922,#15923,#15924,#15925,
#15926,#15927,#15928,#15929,#15930,#15931,#15932,#15933,#15934,#15935,#15936,
#15937,#15938,#15939,#15940,#15941,#15942),.UNSPECIFIED.,.F.,.F.,(4,2,2,
2,2,2,2,2,2,2,4),(0.0473477652366656,0.126350602536658,0.189525903804987,
0.252701205073316,0.313298422430275,0.373895639787233,0.434492857144191,
0.495090074501149,0.558265375769478,0.621440677037807,0.7004435143378),
 .UNSPECIFIED.);
#468=B_SPLINE_CURVE_WITH_KNOTS('',3,(#15951,#15952,#15953,#15954,#15955,
#15956,#15957,#15958,#15959,#15960,#15961,#15962,#15963,#15964,#15965,#15966,
#15967,#15968,#15969,#15970,#15971,#15972),.UNSPECIFIED.,.F.,.F.,(4,2,2,
2,2,2,2,2,2,2,4),(0.0473477652366656,0.126350602536658,0.189525903804987,
0.252701205073317,0.313298422430275,0.373895639787233,0.434492857144191,
0.495090074501149,0.558265375769478,0.621440677037807,0.7004435143378),
 .UNSPECIFIED.);
#469=SPHERICAL_SURFACE('',#9733,2.35);
#470=SPHERICAL_SURFACE('',#9773,2.35);
#471=SPHERICAL_SURFACE('',#10148,0.23815);
#472=SPHERICAL_SURFACE('',#10150,0.23815);
#473=SPHERICAL_SURFACE('',#10152,0.23815);
#474=SPHERICAL_SURFACE('',#10154,0.23815);
#475=SPHERICAL_SURFACE('',#10156,0.23815);
#476=SPHERICAL_SURFACE('',#10158,0.23815);
#477=SPHERICAL_SURFACE('',#10160,0.23815);
#478=SPHERICAL_SURFACE('',#10162,0.23815);
#479=SPHERICAL_SURFACE('',#10165,0.247676);
#480=SPHERICAL_SURFACE('',#10181,0.247676);
#481=SPHERICAL_SURFACE('',#10186,0.247676);
#482=SPHERICAL_SURFACE('',#10191,0.247676);
#483=SPHERICAL_SURFACE('',#10196,0.247676);
#484=SPHERICAL_SURFACE('',#10201,0.247676);
#485=SPHERICAL_SURFACE('',#10206,0.247676);
#486=SPHERICAL_SURFACE('',#10214,0.247676);
#487=SHAPE_REPRESENTATION_RELATIONSHIP('SRR','None',#17126,#537);
#488=SHAPE_REPRESENTATION_RELATIONSHIP('SRR','None',#17127,#538);
#489=SHAPE_REPRESENTATION_RELATIONSHIP('SRR','None',#17128,#539);
#490=SHAPE_REPRESENTATION_RELATIONSHIP('SRR','None',#17129,#540);
#491=SHAPE_REPRESENTATION_RELATIONSHIP('SRR','None',#17130,#541);
#492=SHAPE_REPRESENTATION_RELATIONSHIP('SRR','None',#17131,#542);
#493=SHAPE_REPRESENTATION_RELATIONSHIP('SRR','None',#17132,#543);
#494=SHAPE_REPRESENTATION_RELATIONSHIP('SRR','None',#17133,#544);
#495=SHAPE_REPRESENTATION_RELATIONSHIP('SRR','None',#17134,#545);
#496=SHAPE_REPRESENTATION_RELATIONSHIP('SRR','None',#17135,#546);
#497=SHAPE_REPRESENTATION_RELATIONSHIP('SRR','None',#17137,#547);
#498=SHAPE_REPRESENTATION_RELATIONSHIP('SRR','None',#17138,#548);
#499=SHAPE_REPRESENTATION_RELATIONSHIP('SRR','None',#17139,#549);
#500=SHAPE_REPRESENTATION_RELATIONSHIP('SRR','None',#17140,#550);
#501=SHAPE_REPRESENTATION_RELATIONSHIP('SRR','None',#17141,#551);
#502=SHAPE_REPRESENTATION_RELATIONSHIP('SRR','None',#17142,#552);
#503=SHAPE_REPRESENTATION_RELATIONSHIP('SRR','None',#17144,#553);
#504=SHAPE_REPRESENTATION_RELATIONSHIP('SRR','None',#17145,#554);
#505=SHAPE_REPRESENTATION_RELATIONSHIP('SRR','None',#17146,#555);
#506=SHAPE_REPRESENTATION_RELATIONSHIP('SRR','None',#17147,#556);
#507=SHAPE_REPRESENTATION_RELATIONSHIP('SRR','None',#17148,#557);
#508=SHAPE_REPRESENTATION_RELATIONSHIP('SRR','None',#17149,#558);
#509=SHAPE_REPRESENTATION_RELATIONSHIP('SRR','None',#17150,#559);
#510=SHAPE_REPRESENTATION_RELATIONSHIP('SRR','None',#17151,#560);
#511=SHAPE_REPRESENTATION_RELATIONSHIP('SRR','None',#17152,#561);
#512=SHAPE_REPRESENTATION_RELATIONSHIP('SRR','None',#17153,#562);
#513=SHAPE_REPRESENTATION_RELATIONSHIP('SRR','None',#17154,#563);
#514=SHAPE_REPRESENTATION_RELATIONSHIP('SRR','None',#17156,#564);
#515=SHAPE_REPRESENTATION_RELATIONSHIP('SRR','None',#17157,#565);
#516=SHAPE_REPRESENTATION_RELATIONSHIP('SRR','None',#17158,#566);
#517=SHAPE_REPRESENTATION_RELATIONSHIP('SRR','None',#17159,#567);
#518=SHAPE_REPRESENTATION_RELATIONSHIP('SRR','None',#17160,#568);
#519=SHAPE_REPRESENTATION_RELATIONSHIP('SRR','None',#17162,#569);
#520=SHAPE_REPRESENTATION_RELATIONSHIP('SRR','None',#17163,#570);
#521=SHAPE_REPRESENTATION_RELATIONSHIP('SRR','None',#17164,#571);
#522=SHAPE_REPRESENTATION_RELATIONSHIP('SRR','None',#17165,#572);
#523=SHAPE_REPRESENTATION_RELATIONSHIP('SRR','None',#17166,#573);
#524=SHAPE_REPRESENTATION_RELATIONSHIP('SRR','None',#17168,#574);
#525=SHAPE_REPRESENTATION_RELATIONSHIP('SRR','None',#17169,#575);
#526=SHAPE_REPRESENTATION_RELATIONSHIP('SRR','None',#17170,#576);
#527=SHAPE_REPRESENTATION_RELATIONSHIP('SRR','None',#17171,#577);
#528=SHAPE_REPRESENTATION_RELATIONSHIP('SRR','None',#17172,#578);
#529=SHAPE_REPRESENTATION_RELATIONSHIP('SRR','None',#17173,#579);
#530=SHAPE_REPRESENTATION_RELATIONSHIP('SRR','None',#17175,#580);
#531=SHAPE_REPRESENTATION_RELATIONSHIP('SRR','None',#17176,#581);
#532=SHAPE_REPRESENTATION_RELATIONSHIP('SRR','None',#17177,#582);
#533=SHAPE_REPRESENTATION_RELATIONSHIP('SRR','None',#17178,#583);
#534=SHAPE_REPRESENTATION_RELATIONSHIP('SRR','None',#17179,#584);
#535=SHAPE_REPRESENTATION_RELATIONSHIP('SRR','None',#17180,#585);
#536=SHAPE_REPRESENTATION_RELATIONSHIP('SRR','None',#17181,#586);
#537=ADVANCED_BREP_SHAPE_REPRESENTATION('',(#646),#16855);
#538=ADVANCED_BREP_SHAPE_REPRESENTATION('',(#647),#16856);
#539=ADVANCED_BREP_SHAPE_REPRESENTATION('',(#648),#16857);
#540=ADVANCED_BREP_SHAPE_REPRESENTATION('',(#649),#16858);
#541=ADVANCED_BREP_SHAPE_REPRESENTATION('',(#650),#16859);
#542=ADVANCED_BREP_SHAPE_REPRESENTATION('',(#651),#16860);
#543=ADVANCED_BREP_SHAPE_REPRESENTATION('',(#652),#16861);
#544=ADVANCED_BREP_SHAPE_REPRESENTATION('',(#653),#16862);
#545=ADVANCED_BREP_SHAPE_REPRESENTATION('',(#654),#16863);
#546=ADVANCED_BREP_SHAPE_REPRESENTATION('',(#655),#16864);
#547=ADVANCED_BREP_SHAPE_REPRESENTATION('',(#656),#16866);
#548=ADVANCED_BREP_SHAPE_REPRESENTATION('',(#657,#658),#16867);
#549=ADVANCED_BREP_SHAPE_REPRESENTATION('',(#659),#16868);
#550=ADVANCED_BREP_SHAPE_REPRESENTATION('',(#42),#16869);
#551=ADVANCED_BREP_SHAPE_REPRESENTATION('',(#660),#16870);
#552=ADVANCED_BREP_SHAPE_REPRESENTATION('',(#43),#16871);
#553=ADVANCED_BREP_SHAPE_REPRESENTATION('',(#661),#16873);
#554=ADVANCED_BREP_SHAPE_REPRESENTATION('',(#662),#16874);
#555=ADVANCED_BREP_SHAPE_REPRESENTATION('',(#663),#16875);
#556=ADVANCED_BREP_SHAPE_REPRESENTATION('',(#664),#16876);
#557=ADVANCED_BREP_SHAPE_REPRESENTATION('',(#665),#16877);
#558=ADVANCED_BREP_SHAPE_REPRESENTATION('',(#666),#16878);
#559=ADVANCED_BREP_SHAPE_REPRESENTATION('',(#667),#16879);
#560=ADVANCED_BREP_SHAPE_REPRESENTATION('',(#668),#16880);
#561=ADVANCED_BREP_SHAPE_REPRESENTATION('',(#669),#16881);
#562=ADVANCED_BREP_SHAPE_REPRESENTATION('',(#670),#16882);
#563=ADVANCED_BREP_SHAPE_REPRESENTATION('',(#671),#16883);
#564=ADVANCED_BREP_SHAPE_REPRESENTATION('',(#672),#16885);
#565=ADVANCED_BREP_SHAPE_REPRESENTATION('',(#673),#16886);
#566=ADVANCED_BREP_SHAPE_REPRESENTATION('',(#674),#16887);
#567=ADVANCED_BREP_SHAPE_REPRESENTATION('',(#675),#16888);
#568=ADVANCED_BREP_SHAPE_REPRESENTATION('',(#676),#16889);
#569=ADVANCED_BREP_SHAPE_REPRESENTATION('',(#677),#16891);
#570=ADVANCED_BREP_SHAPE_REPRESENTATION('',(#678),#16892);
#571=ADVANCED_BREP_SHAPE_REPRESENTATION('',(#679,#680,#681,#682,#683,#684,
#685,#686),#16893);
#572=ADVANCED_BREP_SHAPE_REPRESENTATION('',(#687),#16894);
#573=ADVANCED_BREP_SHAPE_REPRESENTATION('',(#688,#689),#16895);
#574=ADVANCED_BREP_SHAPE_REPRESENTATION('',(#690),#16897);
#575=ADVANCED_BREP_SHAPE_REPRESENTATION('',(#691),#16898);
#576=ADVANCED_BREP_SHAPE_REPRESENTATION('',(#692),#16899);
#577=ADVANCED_BREP_SHAPE_REPRESENTATION('',(#693),#16900);
#578=ADVANCED_BREP_SHAPE_REPRESENTATION('',(#694),#16901);
#579=ADVANCED_BREP_SHAPE_REPRESENTATION('',(#695),#16902);
#580=ADVANCED_BREP_SHAPE_REPRESENTATION('',(#696),#16904);
#581=ADVANCED_BREP_SHAPE_REPRESENTATION('',(#697),#16905);
#582=ADVANCED_BREP_SHAPE_REPRESENTATION('',(#698),#16906);
#583=ADVANCED_BREP_SHAPE_REPRESENTATION('',(#44),#16907);
#584=ADVANCED_BREP_SHAPE_REPRESENTATION('',(#699),#16908);
#585=ADVANCED_BREP_SHAPE_REPRESENTATION('',(#45),#16909);
#586=ADVANCED_BREP_SHAPE_REPRESENTATION('',(#46),#16910);
#587=STYLED_ITEM('',(#17466),#646);
#588=STYLED_ITEM('',(#17487),#647);
#589=STYLED_ITEM('',(#17494),#648);
#590=STYLED_ITEM('',(#17494),#649);
#591=STYLED_ITEM('',(#17487),#650);
#592=STYLED_ITEM('',(#17494),#651);
#593=STYLED_ITEM('',(#17494),#652);
#594=STYLED_ITEM('',(#17501),#653);
#595=STYLED_ITEM('',(#17473),#654);
#596=STYLED_ITEM('',(#17473),#655);
#597=STYLED_ITEM('',(#17466),#656);
#598=STYLED_ITEM('',(#17487),#657);
#599=STYLED_ITEM('',(#17487),#658);
#600=STYLED_ITEM('',(#17494),#659);
#601=STYLED_ITEM('',(#17494),#42);
#602=STYLED_ITEM('',(#17480),#660);
#603=STYLED_ITEM('',(#17494),#43);
#604=STYLED_ITEM('',(#17487),#661);
#605=STYLED_ITEM('',(#17487),#662);
#606=STYLED_ITEM('',(#17487),#663);
#607=STYLED_ITEM('',(#17487),#664);
#608=STYLED_ITEM('',(#17501),#665);
#609=STYLED_ITEM('',(#17487),#666);
#610=STYLED_ITEM('',(#17487),#667);
#611=STYLED_ITEM('',(#17487),#668);
#612=STYLED_ITEM('',(#17487),#669);
#613=STYLED_ITEM('',(#17487),#670);
#614=STYLED_ITEM('',(#17494),#671);
#615=STYLED_ITEM('',(#17487),#672);
#616=STYLED_ITEM('',(#17487),#673);
#617=STYLED_ITEM('',(#17487),#674);
#618=STYLED_ITEM('',(#17487),#675);
#619=STYLED_ITEM('',(#17487),#676);
#620=STYLED_ITEM('',(#17487),#677);
#621=STYLED_ITEM('',(#17487),#678);
#622=STYLED_ITEM('',(#17487),#679);
#623=STYLED_ITEM('',(#17487),#680);
#624=STYLED_ITEM('',(#17487),#681);
#625=STYLED_ITEM('',(#17487),#682);
#626=STYLED_ITEM('',(#17487),#683);
#627=STYLED_ITEM('',(#17487),#684);
#628=STYLED_ITEM('',(#17487),#685);
#629=STYLED_ITEM('',(#17487),#686);
#630=STYLED_ITEM('',(#17487),#687);
#631=STYLED_ITEM('',(#17487),#688);
#632=STYLED_ITEM('',(#17487),#689);
#633=STYLED_ITEM('',(#17501),#690);
#634=STYLED_ITEM('',(#17480),#691);
#635=STYLED_ITEM('',(#17487),#692);
#636=STYLED_ITEM('',(#17487),#693);
#637=STYLED_ITEM('',(#17487),#694);
#638=STYLED_ITEM('',(#17487),#695);
#639=STYLED_ITEM('',(#17466),#696);
#640=STYLED_ITEM('',(#17480),#697);
#641=STYLED_ITEM('',(#17501),#698);
#642=STYLED_ITEM('',(#17494),#44);
#643=STYLED_ITEM('',(#17494),#699);
#644=STYLED_ITEM('',(#17494),#45);
#645=STYLED_ITEM('',(#17494),#46);
#646=MANIFOLD_SOLID_BREP('Body1',#8878);
#647=MANIFOLD_SOLID_BREP('Body1',#8879);
#648=MANIFOLD_SOLID_BREP('Body1',#8880);
#649=MANIFOLD_SOLID_BREP('Body1',#8881);
#650=MANIFOLD_SOLID_BREP('Body1',#8882);
#651=MANIFOLD_SOLID_BREP('Body1',#8883);
#652=MANIFOLD_SOLID_BREP('Body1',#8884);
#653=MANIFOLD_SOLID_BREP('Body1',#8885);
#654=MANIFOLD_SOLID_BREP('Body1',#8886);
#655=MANIFOLD_SOLID_BREP('Body1',#8887);
#656=MANIFOLD_SOLID_BREP('Body1',#8888);
#657=MANIFOLD_SOLID_BREP('Body1',#8889);
#658=MANIFOLD_SOLID_BREP('Body2',#8890);
#659=MANIFOLD_SOLID_BREP('Body1',#8891);
#660=MANIFOLD_SOLID_BREP('Body1',#8894);
#661=MANIFOLD_SOLID_BREP('Body1',#8897);
#662=MANIFOLD_SOLID_BREP('Body1',#8898);
#663=MANIFOLD_SOLID_BREP('Body1',#8899);
#664=MANIFOLD_SOLID_BREP('Body1',#8900);
#665=MANIFOLD_SOLID_BREP('Body1',#8901);
#666=MANIFOLD_SOLID_BREP('Body1',#8902);
#667=MANIFOLD_SOLID_BREP('Body1',#8903);
#668=MANIFOLD_SOLID_BREP('Body1',#8904);
#669=MANIFOLD_SOLID_BREP('Body1',#8905);
#670=MANIFOLD_SOLID_BREP('Body1',#8906);
#671=MANIFOLD_SOLID_BREP('Body1',#8907);
#672=MANIFOLD_SOLID_BREP('Body1',#8908);
#673=MANIFOLD_SOLID_BREP('Body1',#8909);
#674=MANIFOLD_SOLID_BREP('Body1',#8910);
#675=MANIFOLD_SOLID_BREP('Body1',#8911);
#676=MANIFOLD_SOLID_BREP('Body1',#8912);
#677=MANIFOLD_SOLID_BREP('Body1',#8913);
#678=MANIFOLD_SOLID_BREP('Body1',#8914);
#679=MANIFOLD_SOLID_BREP('Body1',#8915);
#680=MANIFOLD_SOLID_BREP('Body2',#8916);
#681=MANIFOLD_SOLID_BREP('Body3',#8917);
#682=MANIFOLD_SOLID_BREP('Body4',#8918);
#683=MANIFOLD_SOLID_BREP('Body5',#8919);
#684=MANIFOLD_SOLID_BREP('Body6',#8920);
#685=MANIFOLD_SOLID_BREP('Body7',#8921);
#686=MANIFOLD_SOLID_BREP('Body8',#8922);
#687=MANIFOLD_SOLID_BREP('Continuous crown cage',#8923);
#688=MANIFOLD_SOLID_BREP('Body1',#8924);
#689=MANIFOLD_SOLID_BREP('Body2',#8925);
#690=MANIFOLD_SOLID_BREP('Body1',#8926);
#691=MANIFOLD_SOLID_BREP('Body1',#8927);
#692=MANIFOLD_SOLID_BREP('Body1',#8928);
#693=MANIFOLD_SOLID_BREP('Body1',#8929);
#694=MANIFOLD_SOLID_BREP('Body1',#8930);
#695=MANIFOLD_SOLID_BREP('Body1',#8931);
#696=MANIFOLD_SOLID_BREP('Body1',#8932);
#697=MANIFOLD_SOLID_BREP('Body1',#8933);
#698=MANIFOLD_SOLID_BREP('Body1',#8934);
#699=MANIFOLD_SOLID_BREP('Body1',#8937);
#700=FACE_BOUND('',#1757,.T.);
#701=FACE_BOUND('',#1758,.T.);
#702=FACE_BOUND('',#1759,.T.);
#703=FACE_BOUND('',#1760,.T.);
#704=FACE_BOUND('',#1761,.T.);
#705=FACE_BOUND('',#1762,.T.);
#706=FACE_BOUND('',#1763,.T.);
#707=FACE_BOUND('',#1764,.T.);
#708=FACE_BOUND('',#1765,.T.);
#709=FACE_BOUND('',#1766,.T.);
#710=FACE_BOUND('',#1767,.T.);
#711=FACE_BOUND('',#1768,.T.);
#712=FACE_BOUND('',#1770,.T.);
#713=FACE_BOUND('',#1771,.T.);
#714=FACE_BOUND('',#1772,.T.);
#715=FACE_BOUND('',#1773,.T.);
#716=FACE_BOUND('',#1774,.T.);
#717=FACE_BOUND('',#1775,.T.);
#718=FACE_BOUND('',#1776,.T.);
#719=FACE_BOUND('',#1777,.T.);
#720=FACE_BOUND('',#1778,.T.);
#721=FACE_BOUND('',#1779,.T.);
#722=FACE_BOUND('',#1780,.T.);
#723=FACE_BOUND('',#1781,.T.);
#724=FACE_BOUND('',#1788,.T.);
#725=FACE_BOUND('',#1791,.T.);
#726=FACE_BOUND('',#1794,.T.);
#727=FACE_BOUND('',#1797,.T.);
#728=FACE_BOUND('',#1807,.T.);
#729=FACE_BOUND('',#1808,.T.);
#730=FACE_BOUND('',#1809,.T.);
#731=FACE_BOUND('',#1810,.T.);
#732=FACE_BOUND('',#1811,.T.);
#733=FACE_BOUND('',#1812,.T.);
#734=FACE_BOUND('',#1814,.T.);
#735=FACE_BOUND('',#1815,.T.);
#736=FACE_BOUND('',#1816,.T.);
#737=FACE_BOUND('',#1817,.T.);
#738=FACE_BOUND('',#1821,.T.);
#739=FACE_BOUND('',#1823,.T.);
#740=FACE_BOUND('',#1827,.T.);
#741=FACE_BOUND('',#1829,.T.);
#742=FACE_BOUND('',#1836,.T.);
#743=FACE_BOUND('',#1839,.T.);
#744=FACE_BOUND('',#1842,.T.);
#745=FACE_BOUND('',#1845,.T.);
#746=FACE_BOUND('',#1855,.T.);
#747=FACE_BOUND('',#1856,.T.);
#748=FACE_BOUND('',#1857,.T.);
#749=FACE_BOUND('',#1858,.T.);
#750=FACE_BOUND('',#1859,.T.);
#751=FACE_BOUND('',#1860,.T.);
#752=FACE_BOUND('',#1862,.T.);
#753=FACE_BOUND('',#1863,.T.);
#754=FACE_BOUND('',#1864,.T.);
#755=FACE_BOUND('',#1865,.T.);
#756=FACE_BOUND('',#1869,.T.);
#757=FACE_BOUND('',#1871,.T.);
#758=FACE_BOUND('',#1875,.T.);
#759=FACE_BOUND('',#1877,.T.);
#760=FACE_BOUND('',#1888,.T.);
#761=FACE_BOUND('',#1891,.T.);
#762=FACE_BOUND('',#1894,.T.);
#763=FACE_BOUND('',#1897,.T.);
#764=FACE_BOUND('',#1907,.T.);
#765=FACE_BOUND('',#1908,.T.);
#766=FACE_BOUND('',#1909,.T.);
#767=FACE_BOUND('',#1910,.T.);
#768=FACE_BOUND('',#1911,.T.);
#769=FACE_BOUND('',#1912,.T.);
#770=FACE_BOUND('',#1913,.T.);
#771=FACE_BOUND('',#1914,.T.);
#772=FACE_BOUND('',#1916,.T.);
#773=FACE_BOUND('',#1917,.T.);
#774=FACE_BOUND('',#1918,.T.);
#775=FACE_BOUND('',#1919,.T.);
#776=FACE_BOUND('',#1935,.T.);
#777=FACE_BOUND('',#1936,.T.);
#778=FACE_BOUND('',#1944,.T.);
#779=FACE_BOUND('',#1945,.T.);
#780=FACE_BOUND('',#1946,.T.);
#781=FACE_BOUND('',#1949,.T.);
#782=FACE_BOUND('',#1951,.T.);
#783=FACE_BOUND('',#1964,.T.);
#784=FACE_BOUND('',#1965,.T.);
#785=FACE_BOUND('',#1966,.T.);
#786=FACE_BOUND('',#1969,.T.);
#787=FACE_BOUND('',#1971,.T.);
#788=FACE_BOUND('',#1972,.T.);
#789=FACE_BOUND('',#1974,.T.);
#790=FACE_BOUND('',#1978,.T.);
#791=FACE_BOUND('',#1979,.T.);
#792=FACE_BOUND('',#1980,.T.);
#793=FACE_BOUND('',#1981,.T.);
#794=FACE_BOUND('',#1982,.T.);
#795=FACE_BOUND('',#1983,.T.);
#796=FACE_BOUND('',#1989,.T.);
#797=FACE_BOUND('',#1991,.T.);
#798=FACE_BOUND('',#1994,.T.);
#799=FACE_BOUND('',#1996,.T.);
#800=FACE_BOUND('',#1997,.T.);
#801=FACE_BOUND('',#1998,.T.);
#802=FACE_BOUND('',#1999,.T.);
#803=FACE_BOUND('',#2000,.T.);
#804=FACE_BOUND('',#2001,.T.);
#805=FACE_BOUND('',#2005,.T.);
#806=FACE_BOUND('',#2007,.T.);
#807=FACE_BOUND('',#2022,.T.);
#808=FACE_BOUND('',#2027,.T.);
#809=FACE_BOUND('',#2030,.T.);
#810=FACE_BOUND('',#2033,.T.);
#811=FACE_BOUND('',#2036,.T.);
#812=FACE_BOUND('',#2046,.T.);
#813=FACE_BOUND('',#2047,.T.);
#814=FACE_BOUND('',#2048,.T.);
#815=FACE_BOUND('',#2049,.T.);
#816=FACE_BOUND('',#2056,.T.);
#817=FACE_BOUND('',#2057,.T.);
#818=FACE_BOUND('',#2058,.T.);
#819=FACE_BOUND('',#2059,.T.);
#820=FACE_BOUND('',#2068,.T.);
#821=FACE_BOUND('',#2092,.T.);
#822=FACE_BOUND('',#2094,.T.);
#823=FACE_BOUND('',#2096,.T.);
#824=FACE_BOUND('',#2098,.T.);
#825=FACE_BOUND('',#2103,.T.);
#826=FACE_BOUND('',#2105,.T.);
#827=FACE_BOUND('',#2107,.T.);
#828=FACE_BOUND('',#2109,.T.);
#829=FACE_BOUND('',#2113,.T.);
#830=FACE_BOUND('',#2115,.T.);
#831=FACE_BOUND('',#2121,.T.);
#832=FACE_BOUND('',#2129,.T.);
#833=FACE_BOUND('',#2136,.T.);
#834=FACE_BOUND('',#2139,.T.);
#835=FACE_BOUND('',#2145,.T.);
#836=FACE_BOUND('',#2147,.T.);
#837=FACE_BOUND('',#2151,.T.);
#838=FACE_BOUND('',#2153,.T.);
#839=FACE_BOUND('',#2157,.T.);
#840=FACE_BOUND('',#2159,.T.);
#841=FACE_BOUND('',#2178,.T.);
#842=FACE_BOUND('',#2187,.T.);
#843=FACE_BOUND('',#2188,.T.);
#844=FACE_BOUND('',#2193,.T.);
#845=FACE_BOUND('',#2194,.T.);
#846=FACE_BOUND('',#2198,.T.);
#847=FACE_BOUND('',#2200,.T.);
#848=FACE_BOUND('',#2204,.T.);
#849=FACE_BOUND('',#2206,.T.);
#850=FACE_BOUND('',#2210,.T.);
#851=FACE_BOUND('',#2212,.T.);
#852=FACE_BOUND('',#2216,.T.);
#853=FACE_BOUND('',#2218,.T.);
#854=FACE_BOUND('',#2224,.T.);
#855=FACE_BOUND('',#2227,.T.);
#856=FACE_BOUND('',#2232,.T.);
#857=FACE_BOUND('',#2237,.T.);
#858=FACE_BOUND('',#2265,.T.);
#859=FACE_BOUND('',#2268,.T.);
#860=FACE_BOUND('',#2271,.T.);
#861=FACE_BOUND('',#2274,.T.);
#862=FACE_BOUND('',#2277,.T.);
#863=FACE_BOUND('',#2286,.T.);
#864=FACE_BOUND('',#2287,.T.);
#865=FACE_BOUND('',#2291,.T.);
#866=FACE_BOUND('',#2296,.T.);
#867=FACE_BOUND('',#2306,.T.);
#868=FACE_BOUND('',#2307,.T.);
#869=FACE_BOUND('',#2308,.T.);
#870=FACE_BOUND('',#2309,.T.);
#871=FACE_BOUND('',#2310,.T.);
#872=FACE_BOUND('',#2312,.T.);
#873=FACE_BOUND('',#2313,.T.);
#874=FACE_BOUND('',#2314,.T.);
#875=FACE_BOUND('',#2315,.T.);
#876=FACE_BOUND('',#2323,.T.);
#877=FACE_BOUND('',#2324,.T.);
#878=FACE_BOUND('',#2326,.T.);
#879=FACE_BOUND('',#2327,.T.);
#880=FACE_BOUND('',#2331,.T.);
#881=FACE_BOUND('',#2336,.T.);
#882=FACE_BOUND('',#2340,.T.);
#883=FACE_BOUND('',#2342,.T.);
#884=FACE_BOUND('',#2346,.T.);
#885=FACE_BOUND('',#2348,.T.);
#886=FACE_BOUND('',#2352,.T.);
#887=FACE_BOUND('',#2354,.T.);
#888=FACE_BOUND('',#2369,.T.);
#889=FACE_BOUND('',#2370,.T.);
#890=FACE_BOUND('',#2371,.T.);
#891=FACE_BOUND('',#2372,.T.);
#892=FACE_BOUND('',#2415,.T.);
#893=FACE_BOUND('',#2421,.T.);
#894=FACE_BOUND('',#2424,.T.);
#895=FACE_BOUND('',#2430,.T.);
#896=FACE_BOUND('',#2457,.T.);
#897=PLANE('',#9532);
#898=PLANE('',#9533);
#899=PLANE('',#9534);
#900=PLANE('',#9535);
#901=PLANE('',#9536);
#902=PLANE('',#9537);
#903=PLANE('',#9542);
#904=PLANE('',#9546);
#905=PLANE('',#9550);
#906=PLANE('',#9555);
#907=PLANE('',#9560);
#908=PLANE('',#9565);
#909=PLANE('',#9575);
#910=PLANE('',#9576);
#911=PLANE('',#9577);
#912=PLANE('',#9578);
#913=PLANE('',#9579);
#914=PLANE('',#9580);
#915=PLANE('',#9588);
#916=PLANE('',#9589);
#917=PLANE('',#9597);
#918=PLANE('',#9598);
#919=PLANE('',#9603);
#920=PLANE('',#9607);
#921=PLANE('',#9611);
#922=PLANE('',#9616);
#923=PLANE('',#9621);
#924=PLANE('',#9626);
#925=PLANE('',#9636);
#926=PLANE('',#9637);
#927=PLANE('',#9638);
#928=PLANE('',#9639);
#929=PLANE('',#9640);
#930=PLANE('',#9641);
#931=PLANE('',#9649);
#932=PLANE('',#9650);
#933=PLANE('',#9658);
#934=PLANE('',#9659);
#935=PLANE('',#9664);
#936=PLANE('',#9668);
#937=PLANE('',#9672);
#938=PLANE('',#9676);
#939=PLANE('',#9680);
#940=PLANE('',#9685);
#941=PLANE('',#9690);
#942=PLANE('',#9695);
#943=PLANE('',#9705);
#944=PLANE('',#9706);
#945=PLANE('',#9707);
#946=PLANE('',#9708);
#947=PLANE('',#9709);
#948=PLANE('',#9710);
#949=PLANE('',#9712);
#950=PLANE('',#9713);
#951=PLANE('',#9714);
#952=PLANE('',#9715);
#953=PLANE('',#9716);
#954=PLANE('',#9717);
#955=PLANE('',#9719);
#956=PLANE('',#9720);
#957=PLANE('',#9721);
#958=PLANE('',#9722);
#959=PLANE('',#9723);
#960=PLANE('',#9724);
#961=PLANE('',#9735);
#962=PLANE('',#9737);
#963=PLANE('',#9739);
#964=PLANE('',#9741);
#965=PLANE('',#9742);
#966=PLANE('',#9744);
#967=PLANE('',#9745);
#968=PLANE('',#9751);
#969=PLANE('',#9752);
#970=PLANE('',#9753);
#971=PLANE('',#9754);
#972=PLANE('',#9755);
#973=PLANE('',#9756);
#974=PLANE('',#9757);
#975=PLANE('',#9762);
#976=PLANE('',#9763);
#977=PLANE('',#9764);
#978=PLANE('',#9765);
#979=PLANE('',#9766);
#980=PLANE('',#9771);
#981=PLANE('',#9776);
#982=PLANE('',#9786);
#983=PLANE('',#9788);
#984=PLANE('',#9792);
#985=PLANE('',#9804);
#986=PLANE('',#9805);
#987=PLANE('',#9807);
#988=PLANE('',#9808);
#989=PLANE('',#9809);
#990=PLANE('',#9810);
#991=PLANE('',#9811);
#992=PLANE('',#9812);
#993=PLANE('',#9813);
#994=PLANE('',#9814);
#995=PLANE('',#9815);
#996=PLANE('',#9817);
#997=PLANE('',#9825);
#998=PLANE('',#9834);
#999=PLANE('',#9839);
#1000=PLANE('',#9844);
#1001=PLANE('',#9849);
#1002=PLANE('',#9859);
#1003=PLANE('',#9860);
#1004=PLANE('',#9861);
#1005=PLANE('',#9862);
#1006=PLANE('',#9863);
#1007=PLANE('',#9864);
#1008=PLANE('',#9865);
#1009=PLANE('',#9866);
#1010=PLANE('',#9867);
#1011=PLANE('',#9868);
#1012=PLANE('',#9869);
#1013=PLANE('',#9870);
#1014=PLANE('',#9871);
#1015=PLANE('',#9872);
#1016=PLANE('',#9874);
#1017=PLANE('',#9882);
#1018=PLANE('',#9890);
#1019=PLANE('',#9891);
#1020=PLANE('',#9892);
#1021=PLANE('',#9893);
#1022=PLANE('',#9894);
#1023=PLANE('',#9895);
#1024=PLANE('',#9896);
#1025=PLANE('',#9897);
#1026=PLANE('',#9898);
#1027=PLANE('',#9901);
#1028=PLANE('',#9902);
#1029=PLANE('',#9904);
#1030=PLANE('',#9905);
#1031=PLANE('',#9910);
#1032=PLANE('',#9911);
#1033=PLANE('',#9913);
#1034=PLANE('',#9918);
#1035=PLANE('',#9925);
#1036=PLANE('',#9926);
#1037=PLANE('',#9928);
#1038=PLANE('',#9933);
#1039=PLANE('',#9940);
#1040=PLANE('',#9941);
#1041=PLANE('',#9949);
#1042=PLANE('',#9950);
#1043=PLANE('',#9952);
#1044=PLANE('',#9964);
#1045=PLANE('',#9965);
#1046=PLANE('',#9967);
#1047=PLANE('',#9968);
#1048=PLANE('',#9969);
#1049=PLANE('',#9973);
#1050=PLANE('',#9974);
#1051=PLANE('',#9975);
#1052=PLANE('',#9982);
#1053=PLANE('',#9987);
#1054=PLANE('',#9988);
#1055=PLANE('',#9993);
#1056=PLANE('',#9996);
#1057=PLANE('',#10004);
#1058=PLANE('',#10005);
#1059=PLANE('',#10013);
#1060=PLANE('',#10014);
#1061=PLANE('',#10022);
#1062=PLANE('',#10023);
#1063=PLANE('',#10025);
#1064=PLANE('',#10026);
#1065=PLANE('',#10027);
#1066=PLANE('',#10028);
#1067=PLANE('',#10029);
#1068=PLANE('',#10030);
#1069=PLANE('',#10031);
#1070=PLANE('',#10032);
#1071=PLANE('',#10033);
#1072=PLANE('',#10034);
#1073=PLANE('',#10036);
#1074=PLANE('',#10037);
#1075=PLANE('',#10038);
#1076=PLANE('',#10039);
#1077=PLANE('',#10040);
#1078=PLANE('',#10041);
#1079=PLANE('',#10042);
#1080=PLANE('',#10043);
#1081=PLANE('',#10051);
#1082=PLANE('',#10063);
#1083=PLANE('',#10065);
#1084=PLANE('',#10068);
#1085=PLANE('',#10069);
#1086=PLANE('',#10077);
#1087=PLANE('',#10078);
#1088=PLANE('',#10086);
#1089=PLANE('',#10087);
#1090=PLANE('',#10095);
#1091=PLANE('',#10096);
#1092=PLANE('',#10104);
#1093=PLANE('',#10105);
#1094=PLANE('',#10121);
#1095=PLANE('',#10124);
#1096=PLANE('',#10136);
#1097=PLANE('',#10145);
#1098=PLANE('',#10178);
#1099=PLANE('',#10183);
#1100=PLANE('',#10188);
#1101=PLANE('',#10193);
#1102=PLANE('',#10198);
#1103=PLANE('',#10203);
#1104=PLANE('',#10212);
#1105=PLANE('',#10216);
#1106=PLANE('',#10217);
#1107=PLANE('',#10219);
#1108=PLANE('',#10224);
#1109=PLANE('',#10227);
#1110=PLANE('',#10232);
#1111=PLANE('',#10252);
#1112=PLANE('',#10256);
#1113=PLANE('',#10257);
#1114=PLANE('',#10258);
#1115=PLANE('',#10259);
#1116=PLANE('',#10260);
#1117=PLANE('',#10264);
#1118=PLANE('',#10265);
#1119=PLANE('',#10266);
#1120=PLANE('',#10267);
#1121=PLANE('',#10268);
#1122=PLANE('',#10281);
#1123=PLANE('',#10282);
#1124=PLANE('',#10283);
#1125=PLANE('',#10284);
#1126=PLANE('',#10285);
#1127=PLANE('',#10286);
#1128=PLANE('',#10294);
#1129=PLANE('',#10295);
#1130=PLANE('',#10296);
#1131=PLANE('',#10297);
#1132=PLANE('',#10298);
#1133=PLANE('',#10299);
#1134=PLANE('',#10304);
#1135=PLANE('',#10305);
#1136=PLANE('',#10310);
#1137=PLANE('',#10313);
#1138=PLANE('',#10321);
#1139=PLANE('',#10322);
#1140=PLANE('',#10330);
#1141=PLANE('',#10331);
#1142=PLANE('',#10339);
#1143=PLANE('',#10340);
#1144=PLANE('',#10343);
#1145=PLANE('',#10349);
#1146=PLANE('',#10355);
#1147=PLANE('',#10361);
#1148=PLANE('',#10367);
#1149=PLANE('',#10368);
#1150=PLANE('',#10369);
#1151=PLANE('',#10370);
#1152=PLANE('',#10371);
#1153=PLANE('',#10372);
#1154=PLANE('',#10373);
#1155=PLANE('',#10374);
#1156=PLANE('',#10375);
#1157=PLANE('',#10376);
#1158=PLANE('',#10377);
#1159=PLANE('',#10378);
#1160=PLANE('',#10379);
#1161=PLANE('',#10380);
#1162=PLANE('',#10382);
#1163=PLANE('',#10383);
#1164=PLANE('',#10384);
#1165=PLANE('',#10385);
#1166=PLANE('',#10386);
#1167=PLANE('',#10387);
#1168=PLANE('',#10388);
#1169=PLANE('',#10389);
#1170=PLANE('',#10390);
#1171=PLANE('',#10391);
#1172=PLANE('',#10393);
#1173=PLANE('',#10394);
#1174=PLANE('',#10395);
#1175=PLANE('',#10396);
#1176=PLANE('',#10397);
#1177=PLANE('',#10398);
#1178=PLANE('',#10399);
#1179=PLANE('',#10400);
#1180=PLANE('',#10401);
#1181=PLANE('',#10402);
#1182=PLANE('',#10407);
#1183=PLANE('',#10408);
#1184=PLANE('',#10409);
#1185=PLANE('',#10410);
#1186=PLANE('',#10411);
#1187=PLANE('',#10412);
#1188=PLANE('',#10413);
#1189=PLANE('',#10414);
#1190=PLANE('',#10415);
#1191=PLANE('',#10417);
#1192=PLANE('',#10425);
#1193=PLANE('',#10436);
#1194=PLANE('',#10440);
#1195=PLANE('',#10442);
#1196=PLANE('',#10450);
#1197=PLANE('',#10458);
#1198=PLANE('',#10459);
#1199=PLANE('',#10460);
#1200=PLANE('',#10461);
#1201=PLANE('',#10462);
#1202=PLANE('',#10463);
#1203=PLANE('',#10464);
#1204=PLANE('',#10465);
#1205=PLANE('',#10466);
#1206=PLANE('',#10505);
#1207=PLANE('',#10506);
#1208=PLANE('',#10507);
#1209=PLANE('',#10508);
#1210=PLANE('',#10509);
#1211=PLANE('',#10510);
#1212=PLANE('',#10511);
#1213=PLANE('',#10512);
#1214=PLANE('',#10513);
#1215=PLANE('',#10515);
#1216=PLANE('',#10523);
#1217=FACE_OUTER_BOUND('',#1740,.T.);
#1218=FACE_OUTER_BOUND('',#1741,.T.);
#1219=FACE_OUTER_BOUND('',#1742,.T.);
#1220=FACE_OUTER_BOUND('',#1743,.T.);
#1221=FACE_OUTER_BOUND('',#1744,.T.);
#1222=FACE_OUTER_BOUND('',#1745,.T.);
#1223=FACE_OUTER_BOUND('',#1746,.T.);
#1224=FACE_OUTER_BOUND('',#1747,.T.);
#1225=FACE_OUTER_BOUND('',#1748,.T.);
#1226=FACE_OUTER_BOUND('',#1749,.T.);
#1227=FACE_OUTER_BOUND('',#1750,.T.);
#1228=FACE_OUTER_BOUND('',#1751,.T.);
#1229=FACE_OUTER_BOUND('',#1752,.T.);
#1230=FACE_OUTER_BOUND('',#1753,.T.);
#1231=FACE_OUTER_BOUND('',#1754,.T.);
#1232=FACE_OUTER_BOUND('',#1755,.T.);
#1233=FACE_OUTER_BOUND('',#1756,.T.);
#1234=FACE_OUTER_BOUND('',#1769,.T.);
#1235=FACE_OUTER_BOUND('',#1782,.T.);
#1236=FACE_OUTER_BOUND('',#1783,.T.);
#1237=FACE_OUTER_BOUND('',#1784,.T.);
#1238=FACE_OUTER_BOUND('',#1785,.T.);
#1239=FACE_OUTER_BOUND('',#1786,.T.);
#1240=FACE_OUTER_BOUND('',#1787,.T.);
#1241=FACE_OUTER_BOUND('',#1789,.T.);
#1242=FACE_OUTER_BOUND('',#1790,.T.);
#1243=FACE_OUTER_BOUND('',#1792,.T.);
#1244=FACE_OUTER_BOUND('',#1793,.T.);
#1245=FACE_OUTER_BOUND('',#1795,.T.);
#1246=FACE_OUTER_BOUND('',#1796,.T.);
#1247=FACE_OUTER_BOUND('',#1798,.T.);
#1248=FACE_OUTER_BOUND('',#1799,.T.);
#1249=FACE_OUTER_BOUND('',#1800,.T.);
#1250=FACE_OUTER_BOUND('',#1801,.T.);
#1251=FACE_OUTER_BOUND('',#1802,.T.);
#1252=FACE_OUTER_BOUND('',#1803,.T.);
#1253=FACE_OUTER_BOUND('',#1804,.T.);
#1254=FACE_OUTER_BOUND('',#1805,.T.);
#1255=FACE_OUTER_BOUND('',#1806,.T.);
#1256=FACE_OUTER_BOUND('',#1813,.T.);
#1257=FACE_OUTER_BOUND('',#1818,.T.);
#1258=FACE_OUTER_BOUND('',#1819,.T.);
#1259=FACE_OUTER_BOUND('',#1820,.T.);
#1260=FACE_OUTER_BOUND('',#1822,.T.);
#1261=FACE_OUTER_BOUND('',#1824,.T.);
#1262=FACE_OUTER_BOUND('',#1825,.T.);
#1263=FACE_OUTER_BOUND('',#1826,.T.);
#1264=FACE_OUTER_BOUND('',#1828,.T.);
#1265=FACE_OUTER_BOUND('',#1830,.T.);
#1266=FACE_OUTER_BOUND('',#1831,.T.);
#1267=FACE_OUTER_BOUND('',#1832,.T.);
#1268=FACE_OUTER_BOUND('',#1833,.T.);
#1269=FACE_OUTER_BOUND('',#1834,.T.);
#1270=FACE_OUTER_BOUND('',#1835,.T.);
#1271=FACE_OUTER_BOUND('',#1837,.T.);
#1272=FACE_OUTER_BOUND('',#1838,.T.);
#1273=FACE_OUTER_BOUND('',#1840,.T.);
#1274=FACE_OUTER_BOUND('',#1841,.T.);
#1275=FACE_OUTER_BOUND('',#1843,.T.);
#1276=FACE_OUTER_BOUND('',#1844,.T.);
#1277=FACE_OUTER_BOUND('',#1846,.T.);
#1278=FACE_OUTER_BOUND('',#1847,.T.);
#1279=FACE_OUTER_BOUND('',#1848,.T.);
#1280=FACE_OUTER_BOUND('',#1849,.T.);
#1281=FACE_OUTER_BOUND('',#1850,.T.);
#1282=FACE_OUTER_BOUND('',#1851,.T.);
#1283=FACE_OUTER_BOUND('',#1852,.T.);
#1284=FACE_OUTER_BOUND('',#1853,.T.);
#1285=FACE_OUTER_BOUND('',#1854,.T.);
#1286=FACE_OUTER_BOUND('',#1861,.T.);
#1287=FACE_OUTER_BOUND('',#1866,.T.);
#1288=FACE_OUTER_BOUND('',#1867,.T.);
#1289=FACE_OUTER_BOUND('',#1868,.T.);
#1290=FACE_OUTER_BOUND('',#1870,.T.);
#1291=FACE_OUTER_BOUND('',#1872,.T.);
#1292=FACE_OUTER_BOUND('',#1873,.T.);
#1293=FACE_OUTER_BOUND('',#1874,.T.);
#1294=FACE_OUTER_BOUND('',#1876,.T.);
#1295=FACE_OUTER_BOUND('',#1878,.T.);
#1296=FACE_OUTER_BOUND('',#1879,.T.);
#1297=FACE_OUTER_BOUND('',#1880,.T.);
#1298=FACE_OUTER_BOUND('',#1881,.T.);
#1299=FACE_OUTER_BOUND('',#1882,.T.);
#1300=FACE_OUTER_BOUND('',#1883,.T.);
#1301=FACE_OUTER_BOUND('',#1884,.T.);
#1302=FACE_OUTER_BOUND('',#1885,.T.);
#1303=FACE_OUTER_BOUND('',#1886,.T.);
#1304=FACE_OUTER_BOUND('',#1887,.T.);
#1305=FACE_OUTER_BOUND('',#1889,.T.);
#1306=FACE_OUTER_BOUND('',#1890,.T.);
#1307=FACE_OUTER_BOUND('',#1892,.T.);
#1308=FACE_OUTER_BOUND('',#1893,.T.);
#1309=FACE_OUTER_BOUND('',#1895,.T.);
#1310=FACE_OUTER_BOUND('',#1896,.T.);
#1311=FACE_OUTER_BOUND('',#1898,.T.);
#1312=FACE_OUTER_BOUND('',#1899,.T.);
#1313=FACE_OUTER_BOUND('',#1900,.T.);
#1314=FACE_OUTER_BOUND('',#1901,.T.);
#1315=FACE_OUTER_BOUND('',#1902,.T.);
#1316=FACE_OUTER_BOUND('',#1903,.T.);
#1317=FACE_OUTER_BOUND('',#1904,.T.);
#1318=FACE_OUTER_BOUND('',#1905,.T.);
#1319=FACE_OUTER_BOUND('',#1906,.T.);
#1320=FACE_OUTER_BOUND('',#1915,.T.);
#1321=FACE_OUTER_BOUND('',#1920,.T.);
#1322=FACE_OUTER_BOUND('',#1921,.T.);
#1323=FACE_OUTER_BOUND('',#1922,.T.);
#1324=FACE_OUTER_BOUND('',#1923,.T.);
#1325=FACE_OUTER_BOUND('',#1924,.T.);
#1326=FACE_OUTER_BOUND('',#1925,.T.);
#1327=FACE_OUTER_BOUND('',#1926,.T.);
#1328=FACE_OUTER_BOUND('',#1927,.T.);
#1329=FACE_OUTER_BOUND('',#1928,.T.);
#1330=FACE_OUTER_BOUND('',#1929,.T.);
#1331=FACE_OUTER_BOUND('',#1930,.T.);
#1332=FACE_OUTER_BOUND('',#1931,.T.);
#1333=FACE_OUTER_BOUND('',#1932,.T.);
#1334=FACE_OUTER_BOUND('',#1933,.T.);
#1335=FACE_OUTER_BOUND('',#1934,.T.);
#1336=FACE_OUTER_BOUND('',#1937,.T.);
#1337=FACE_OUTER_BOUND('',#1938,.T.);
#1338=FACE_OUTER_BOUND('',#1939,.T.);
#1339=FACE_OUTER_BOUND('',#1940,.T.);
#1340=FACE_OUTER_BOUND('',#1941,.T.);
#1341=FACE_OUTER_BOUND('',#1942,.T.);
#1342=FACE_OUTER_BOUND('',#1943,.T.);
#1343=FACE_OUTER_BOUND('',#1947,.T.);
#1344=FACE_OUTER_BOUND('',#1948,.T.);
#1345=FACE_OUTER_BOUND('',#1950,.T.);
#1346=FACE_OUTER_BOUND('',#1952,.T.);
#1347=FACE_OUTER_BOUND('',#1953,.T.);
#1348=FACE_OUTER_BOUND('',#1954,.T.);
#1349=FACE_OUTER_BOUND('',#1955,.T.);
#1350=FACE_OUTER_BOUND('',#1956,.T.);
#1351=FACE_OUTER_BOUND('',#1957,.T.);
#1352=FACE_OUTER_BOUND('',#1958,.T.);
#1353=FACE_OUTER_BOUND('',#1959,.T.);
#1354=FACE_OUTER_BOUND('',#1960,.T.);
#1355=FACE_OUTER_BOUND('',#1961,.T.);
#1356=FACE_OUTER_BOUND('',#1962,.T.);
#1357=FACE_OUTER_BOUND('',#1963,.T.);
#1358=FACE_OUTER_BOUND('',#1967,.T.);
#1359=FACE_OUTER_BOUND('',#1968,.T.);
#1360=FACE_OUTER_BOUND('',#1970,.T.);
#1361=FACE_OUTER_BOUND('',#1973,.T.);
#1362=FACE_OUTER_BOUND('',#1975,.T.);
#1363=FACE_OUTER_BOUND('',#1976,.T.);
#1364=FACE_OUTER_BOUND('',#1977,.T.);
#1365=FACE_OUTER_BOUND('',#1984,.T.);
#1366=FACE_OUTER_BOUND('',#1985,.T.);
#1367=FACE_OUTER_BOUND('',#1986,.T.);
#1368=FACE_OUTER_BOUND('',#1987,.T.);
#1369=FACE_OUTER_BOUND('',#1988,.T.);
#1370=FACE_OUTER_BOUND('',#1990,.T.);
#1371=FACE_OUTER_BOUND('',#1992,.T.);
#1372=FACE_OUTER_BOUND('',#1993,.T.);
#1373=FACE_OUTER_BOUND('',#1995,.T.);
#1374=FACE_OUTER_BOUND('',#2002,.T.);
#1375=FACE_OUTER_BOUND('',#2003,.T.);
#1376=FACE_OUTER_BOUND('',#2004,.T.);
#1377=FACE_OUTER_BOUND('',#2006,.T.);
#1378=FACE_OUTER_BOUND('',#2008,.T.);
#1379=FACE_OUTER_BOUND('',#2009,.T.);
#1380=FACE_OUTER_BOUND('',#2010,.T.);
#1381=FACE_OUTER_BOUND('',#2011,.T.);
#1382=FACE_OUTER_BOUND('',#2012,.T.);
#1383=FACE_OUTER_BOUND('',#2013,.T.);
#1384=FACE_OUTER_BOUND('',#2014,.T.);
#1385=FACE_OUTER_BOUND('',#2015,.T.);
#1386=FACE_OUTER_BOUND('',#2016,.T.);
#1387=FACE_OUTER_BOUND('',#2017,.T.);
#1388=FACE_OUTER_BOUND('',#2018,.T.);
#1389=FACE_OUTER_BOUND('',#2019,.T.);
#1390=FACE_OUTER_BOUND('',#2020,.T.);
#1391=FACE_OUTER_BOUND('',#2021,.T.);
#1392=FACE_OUTER_BOUND('',#2023,.T.);
#1393=FACE_OUTER_BOUND('',#2024,.T.);
#1394=FACE_OUTER_BOUND('',#2025,.T.);
#1395=FACE_OUTER_BOUND('',#2026,.T.);
#1396=FACE_OUTER_BOUND('',#2028,.T.);
#1397=FACE_OUTER_BOUND('',#2029,.T.);
#1398=FACE_OUTER_BOUND('',#2031,.T.);
#1399=FACE_OUTER_BOUND('',#2032,.T.);
#1400=FACE_OUTER_BOUND('',#2034,.T.);
#1401=FACE_OUTER_BOUND('',#2035,.T.);
#1402=FACE_OUTER_BOUND('',#2037,.T.);
#1403=FACE_OUTER_BOUND('',#2038,.T.);
#1404=FACE_OUTER_BOUND('',#2039,.T.);
#1405=FACE_OUTER_BOUND('',#2040,.T.);
#1406=FACE_OUTER_BOUND('',#2041,.T.);
#1407=FACE_OUTER_BOUND('',#2042,.T.);
#1408=FACE_OUTER_BOUND('',#2043,.T.);
#1409=FACE_OUTER_BOUND('',#2044,.T.);
#1410=FACE_OUTER_BOUND('',#2045,.T.);
#1411=FACE_OUTER_BOUND('',#2050,.T.);
#1412=FACE_OUTER_BOUND('',#2051,.T.);
#1413=FACE_OUTER_BOUND('',#2052,.T.);
#1414=FACE_OUTER_BOUND('',#2053,.T.);
#1415=FACE_OUTER_BOUND('',#2054,.T.);
#1416=FACE_OUTER_BOUND('',#2055,.T.);
#1417=FACE_OUTER_BOUND('',#2060,.T.);
#1418=FACE_OUTER_BOUND('',#2061,.T.);
#1419=FACE_OUTER_BOUND('',#2062,.T.);
#1420=FACE_OUTER_BOUND('',#2063,.T.);
#1421=FACE_OUTER_BOUND('',#2064,.T.);
#1422=FACE_OUTER_BOUND('',#2065,.T.);
#1423=FACE_OUTER_BOUND('',#2066,.T.);
#1424=FACE_OUTER_BOUND('',#2067,.T.);
#1425=FACE_OUTER_BOUND('',#2069,.T.);
#1426=FACE_OUTER_BOUND('',#2070,.T.);
#1427=FACE_OUTER_BOUND('',#2071,.T.);
#1428=FACE_OUTER_BOUND('',#2072,.T.);
#1429=FACE_OUTER_BOUND('',#2073,.T.);
#1430=FACE_OUTER_BOUND('',#2074,.T.);
#1431=FACE_OUTER_BOUND('',#2075,.T.);
#1432=FACE_OUTER_BOUND('',#2076,.T.);
#1433=FACE_OUTER_BOUND('',#2077,.T.);
#1434=FACE_OUTER_BOUND('',#2078,.T.);
#1435=FACE_OUTER_BOUND('',#2079,.T.);
#1436=FACE_OUTER_BOUND('',#2080,.T.);
#1437=FACE_OUTER_BOUND('',#2081,.T.);
#1438=FACE_OUTER_BOUND('',#2082,.T.);
#1439=FACE_OUTER_BOUND('',#2083,.T.);
#1440=FACE_OUTER_BOUND('',#2084,.T.);
#1441=FACE_OUTER_BOUND('',#2085,.T.);
#1442=FACE_OUTER_BOUND('',#2086,.T.);
#1443=FACE_OUTER_BOUND('',#2087,.T.);
#1444=FACE_OUTER_BOUND('',#2088,.T.);
#1445=FACE_OUTER_BOUND('',#2089,.T.);
#1446=FACE_OUTER_BOUND('',#2090,.T.);
#1447=FACE_OUTER_BOUND('',#2091,.T.);
#1448=FACE_OUTER_BOUND('',#2093,.T.);
#1449=FACE_OUTER_BOUND('',#2095,.T.);
#1450=FACE_OUTER_BOUND('',#2097,.T.);
#1451=FACE_OUTER_BOUND('',#2099,.T.);
#1452=FACE_OUTER_BOUND('',#2100,.T.);
#1453=FACE_OUTER_BOUND('',#2101,.T.);
#1454=FACE_OUTER_BOUND('',#2102,.T.);
#1455=FACE_OUTER_BOUND('',#2104,.T.);
#1456=FACE_OUTER_BOUND('',#2106,.T.);
#1457=FACE_OUTER_BOUND('',#2108,.T.);
#1458=FACE_OUTER_BOUND('',#2110,.T.);
#1459=FACE_OUTER_BOUND('',#2111,.T.);
#1460=FACE_OUTER_BOUND('',#2112,.T.);
#1461=FACE_OUTER_BOUND('',#2114,.T.);
#1462=FACE_OUTER_BOUND('',#2116,.T.);
#1463=FACE_OUTER_BOUND('',#2117,.T.);
#1464=FACE_OUTER_BOUND('',#2118,.T.);
#1465=FACE_OUTER_BOUND('',#2119,.T.);
#1466=FACE_OUTER_BOUND('',#2120,.T.);
#1467=FACE_OUTER_BOUND('',#2122,.T.);
#1468=FACE_OUTER_BOUND('',#2123,.T.);
#1469=FACE_OUTER_BOUND('',#2124,.T.);
#1470=FACE_OUTER_BOUND('',#2125,.T.);
#1471=FACE_OUTER_BOUND('',#2126,.T.);
#1472=FACE_OUTER_BOUND('',#2127,.T.);
#1473=FACE_OUTER_BOUND('',#2128,.T.);
#1474=FACE_OUTER_BOUND('',#2130,.T.);
#1475=FACE_OUTER_BOUND('',#2131,.T.);
#1476=FACE_OUTER_BOUND('',#2132,.T.);
#1477=FACE_OUTER_BOUND('',#2133,.T.);
#1478=FACE_OUTER_BOUND('',#2134,.T.);
#1479=FACE_OUTER_BOUND('',#2135,.T.);
#1480=FACE_OUTER_BOUND('',#2137,.T.);
#1481=FACE_OUTER_BOUND('',#2138,.T.);
#1482=FACE_OUTER_BOUND('',#2140,.T.);
#1483=FACE_OUTER_BOUND('',#2141,.T.);
#1484=FACE_OUTER_BOUND('',#2142,.T.);
#1485=FACE_OUTER_BOUND('',#2143,.T.);
#1486=FACE_OUTER_BOUND('',#2144,.T.);
#1487=FACE_OUTER_BOUND('',#2146,.T.);
#1488=FACE_OUTER_BOUND('',#2148,.T.);
#1489=FACE_OUTER_BOUND('',#2149,.T.);
#1490=FACE_OUTER_BOUND('',#2150,.T.);
#1491=FACE_OUTER_BOUND('',#2152,.T.);
#1492=FACE_OUTER_BOUND('',#2154,.T.);
#1493=FACE_OUTER_BOUND('',#2155,.T.);
#1494=FACE_OUTER_BOUND('',#2156,.T.);
#1495=FACE_OUTER_BOUND('',#2158,.T.);
#1496=FACE_OUTER_BOUND('',#2160,.T.);
#1497=FACE_OUTER_BOUND('',#2161,.T.);
#1498=FACE_OUTER_BOUND('',#2162,.T.);
#1499=FACE_OUTER_BOUND('',#2163,.T.);
#1500=FACE_OUTER_BOUND('',#2164,.T.);
#1501=FACE_OUTER_BOUND('',#2165,.T.);
#1502=FACE_OUTER_BOUND('',#2166,.T.);
#1503=FACE_OUTER_BOUND('',#2167,.T.);
#1504=FACE_OUTER_BOUND('',#2168,.T.);
#1505=FACE_OUTER_BOUND('',#2169,.T.);
#1506=FACE_OUTER_BOUND('',#2170,.T.);
#1507=FACE_OUTER_BOUND('',#2171,.T.);
#1508=FACE_OUTER_BOUND('',#2172,.T.);
#1509=FACE_OUTER_BOUND('',#2173,.T.);
#1510=FACE_OUTER_BOUND('',#2174,.T.);
#1511=FACE_OUTER_BOUND('',#2175,.T.);
#1512=FACE_OUTER_BOUND('',#2176,.T.);
#1513=FACE_OUTER_BOUND('',#2177,.T.);
#1514=FACE_OUTER_BOUND('',#2179,.T.);
#1515=FACE_OUTER_BOUND('',#2180,.T.);
#1516=FACE_OUTER_BOUND('',#2181,.T.);
#1517=FACE_OUTER_BOUND('',#2182,.T.);
#1518=FACE_OUTER_BOUND('',#2183,.T.);
#1519=FACE_OUTER_BOUND('',#2184,.T.);
#1520=FACE_OUTER_BOUND('',#2185,.T.);
#1521=FACE_OUTER_BOUND('',#2186,.T.);
#1522=FACE_OUTER_BOUND('',#2189,.T.);
#1523=FACE_OUTER_BOUND('',#2190,.T.);
#1524=FACE_OUTER_BOUND('',#2191,.T.);
#1525=FACE_OUTER_BOUND('',#2192,.T.);
#1526=FACE_OUTER_BOUND('',#2195,.T.);
#1527=FACE_OUTER_BOUND('',#2196,.T.);
#1528=FACE_OUTER_BOUND('',#2197,.T.);
#1529=FACE_OUTER_BOUND('',#2199,.T.);
#1530=FACE_OUTER_BOUND('',#2201,.T.);
#1531=FACE_OUTER_BOUND('',#2202,.T.);
#1532=FACE_OUTER_BOUND('',#2203,.T.);
#1533=FACE_OUTER_BOUND('',#2205,.T.);
#1534=FACE_OUTER_BOUND('',#2207,.T.);
#1535=FACE_OUTER_BOUND('',#2208,.T.);
#1536=FACE_OUTER_BOUND('',#2209,.T.);
#1537=FACE_OUTER_BOUND('',#2211,.T.);
#1538=FACE_OUTER_BOUND('',#2213,.T.);
#1539=FACE_OUTER_BOUND('',#2214,.T.);
#1540=FACE_OUTER_BOUND('',#2215,.T.);
#1541=FACE_OUTER_BOUND('',#2217,.T.);
#1542=FACE_OUTER_BOUND('',#2219,.T.);
#1543=FACE_OUTER_BOUND('',#2220,.T.);
#1544=FACE_OUTER_BOUND('',#2221,.T.);
#1545=FACE_OUTER_BOUND('',#2222,.T.);
#1546=FACE_OUTER_BOUND('',#2223,.T.);
#1547=FACE_OUTER_BOUND('',#2225,.T.);
#1548=FACE_OUTER_BOUND('',#2226,.T.);
#1549=FACE_OUTER_BOUND('',#2228,.T.);
#1550=FACE_OUTER_BOUND('',#2229,.T.);
#1551=FACE_OUTER_BOUND('',#2230,.T.);
#1552=FACE_OUTER_BOUND('',#2231,.T.);
#1553=FACE_OUTER_BOUND('',#2233,.T.);
#1554=FACE_OUTER_BOUND('',#2234,.T.);
#1555=FACE_OUTER_BOUND('',#2235,.T.);
#1556=FACE_OUTER_BOUND('',#2236,.T.);
#1557=FACE_OUTER_BOUND('',#2238,.T.);
#1558=FACE_OUTER_BOUND('',#2239,.T.);
#1559=FACE_OUTER_BOUND('',#2240,.T.);
#1560=FACE_OUTER_BOUND('',#2241,.T.);
#1561=FACE_OUTER_BOUND('',#2242,.T.);
#1562=FACE_OUTER_BOUND('',#2243,.T.);
#1563=FACE_OUTER_BOUND('',#2244,.T.);
#1564=FACE_OUTER_BOUND('',#2245,.T.);
#1565=FACE_OUTER_BOUND('',#2246,.T.);
#1566=FACE_OUTER_BOUND('',#2247,.T.);
#1567=FACE_OUTER_BOUND('',#2248,.T.);
#1568=FACE_OUTER_BOUND('',#2249,.T.);
#1569=FACE_OUTER_BOUND('',#2250,.T.);
#1570=FACE_OUTER_BOUND('',#2251,.T.);
#1571=FACE_OUTER_BOUND('',#2252,.T.);
#1572=FACE_OUTER_BOUND('',#2253,.T.);
#1573=FACE_OUTER_BOUND('',#2254,.T.);
#1574=FACE_OUTER_BOUND('',#2255,.T.);
#1575=FACE_OUTER_BOUND('',#2256,.T.);
#1576=FACE_OUTER_BOUND('',#2257,.T.);
#1577=FACE_OUTER_BOUND('',#2258,.T.);
#1578=FACE_OUTER_BOUND('',#2259,.T.);
#1579=FACE_OUTER_BOUND('',#2260,.T.);
#1580=FACE_OUTER_BOUND('',#2261,.T.);
#1581=FACE_OUTER_BOUND('',#2262,.T.);
#1582=FACE_OUTER_BOUND('',#2263,.T.);
#1583=FACE_OUTER_BOUND('',#2264,.T.);
#1584=FACE_OUTER_BOUND('',#2266,.T.);
#1585=FACE_OUTER_BOUND('',#2267,.T.);
#1586=FACE_OUTER_BOUND('',#2269,.T.);
#1587=FACE_OUTER_BOUND('',#2270,.T.);
#1588=FACE_OUTER_BOUND('',#2272,.T.);
#1589=FACE_OUTER_BOUND('',#2273,.T.);
#1590=FACE_OUTER_BOUND('',#2275,.T.);
#1591=FACE_OUTER_BOUND('',#2276,.T.);
#1592=FACE_OUTER_BOUND('',#2278,.T.);
#1593=FACE_OUTER_BOUND('',#2279,.T.);
#1594=FACE_OUTER_BOUND('',#2280,.T.);
#1595=FACE_OUTER_BOUND('',#2281,.T.);
#1596=FACE_OUTER_BOUND('',#2282,.T.);
#1597=FACE_OUTER_BOUND('',#2283,.T.);
#1598=FACE_OUTER_BOUND('',#2284,.T.);
#1599=FACE_OUTER_BOUND('',#2285,.T.);
#1600=FACE_OUTER_BOUND('',#2288,.T.);
#1601=FACE_OUTER_BOUND('',#2289,.T.);
#1602=FACE_OUTER_BOUND('',#2290,.T.);
#1603=FACE_OUTER_BOUND('',#2292,.T.);
#1604=FACE_OUTER_BOUND('',#2293,.T.);
#1605=FACE_OUTER_BOUND('',#2294,.T.);
#1606=FACE_OUTER_BOUND('',#2295,.T.);
#1607=FACE_OUTER_BOUND('',#2297,.T.);
#1608=FACE_OUTER_BOUND('',#2298,.T.);
#1609=FACE_OUTER_BOUND('',#2299,.T.);
#1610=FACE_OUTER_BOUND('',#2300,.T.);
#1611=FACE_OUTER_BOUND('',#2301,.T.);
#1612=FACE_OUTER_BOUND('',#2302,.T.);
#1613=FACE_OUTER_BOUND('',#2303,.T.);
#1614=FACE_OUTER_BOUND('',#2304,.T.);
#1615=FACE_OUTER_BOUND('',#2305,.T.);
#1616=FACE_OUTER_BOUND('',#2311,.T.);
#1617=FACE_OUTER_BOUND('',#2316,.T.);
#1618=FACE_OUTER_BOUND('',#2317,.T.);
#1619=FACE_OUTER_BOUND('',#2318,.T.);
#1620=FACE_OUTER_BOUND('',#2319,.T.);
#1621=FACE_OUTER_BOUND('',#2320,.T.);
#1622=FACE_OUTER_BOUND('',#2321,.T.);
#1623=FACE_OUTER_BOUND('',#2322,.T.);
#1624=FACE_OUTER_BOUND('',#2325,.T.);
#1625=FACE_OUTER_BOUND('',#2328,.T.);
#1626=FACE_OUTER_BOUND('',#2329,.T.);
#1627=FACE_OUTER_BOUND('',#2330,.T.);
#1628=FACE_OUTER_BOUND('',#2332,.T.);
#1629=FACE_OUTER_BOUND('',#2333,.T.);
#1630=FACE_OUTER_BOUND('',#2334,.T.);
#1631=FACE_OUTER_BOUND('',#2335,.T.);
#1632=FACE_OUTER_BOUND('',#2337,.T.);
#1633=FACE_OUTER_BOUND('',#2338,.T.);
#1634=FACE_OUTER_BOUND('',#2339,.T.);
#1635=FACE_OUTER_BOUND('',#2341,.T.);
#1636=FACE_OUTER_BOUND('',#2343,.T.);
#1637=FACE_OUTER_BOUND('',#2344,.T.);
#1638=FACE_OUTER_BOUND('',#2345,.T.);
#1639=FACE_OUTER_BOUND('',#2347,.T.);
#1640=FACE_OUTER_BOUND('',#2349,.T.);
#1641=FACE_OUTER_BOUND('',#2350,.T.);
#1642=FACE_OUTER_BOUND('',#2351,.T.);
#1643=FACE_OUTER_BOUND('',#2353,.T.);
#1644=FACE_OUTER_BOUND('',#2355,.T.);
#1645=FACE_OUTER_BOUND('',#2356,.T.);
#1646=FACE_OUTER_BOUND('',#2357,.T.);
#1647=FACE_OUTER_BOUND('',#2358,.T.);
#1648=FACE_OUTER_BOUND('',#2359,.T.);
#1649=FACE_OUTER_BOUND('',#2360,.T.);
#1650=FACE_OUTER_BOUND('',#2361,.T.);
#1651=FACE_OUTER_BOUND('',#2362,.T.);
#1652=FACE_OUTER_BOUND('',#2363,.T.);
#1653=FACE_OUTER_BOUND('',#2364,.T.);
#1654=FACE_OUTER_BOUND('',#2365,.T.);
#1655=FACE_OUTER_BOUND('',#2366,.T.);
#1656=FACE_OUTER_BOUND('',#2367,.T.);
#1657=FACE_OUTER_BOUND('',#2368,.T.);
#1658=FACE_OUTER_BOUND('',#2373,.T.);
#1659=FACE_OUTER_BOUND('',#2374,.T.);
#1660=FACE_OUTER_BOUND('',#2375,.T.);
#1661=FACE_OUTER_BOUND('',#2376,.T.);
#1662=FACE_OUTER_BOUND('',#2377,.T.);
#1663=FACE_OUTER_BOUND('',#2378,.T.);
#1664=FACE_OUTER_BOUND('',#2379,.T.);
#1665=FACE_OUTER_BOUND('',#2380,.T.);
#1666=FACE_OUTER_BOUND('',#2381,.T.);
#1667=FACE_OUTER_BOUND('',#2382,.T.);
#1668=FACE_OUTER_BOUND('',#2383,.T.);
#1669=FACE_OUTER_BOUND('',#2384,.T.);
#1670=FACE_OUTER_BOUND('',#2385,.T.);
#1671=FACE_OUTER_BOUND('',#2386,.T.);
#1672=FACE_OUTER_BOUND('',#2387,.T.);
#1673=FACE_OUTER_BOUND('',#2388,.T.);
#1674=FACE_OUTER_BOUND('',#2389,.T.);
#1675=FACE_OUTER_BOUND('',#2390,.T.);
#1676=FACE_OUTER_BOUND('',#2391,.T.);
#1677=FACE_OUTER_BOUND('',#2392,.T.);
#1678=FACE_OUTER_BOUND('',#2393,.T.);
#1679=FACE_OUTER_BOUND('',#2394,.T.);
#1680=FACE_OUTER_BOUND('',#2395,.T.);
#1681=FACE_OUTER_BOUND('',#2396,.T.);
#1682=FACE_OUTER_BOUND('',#2397,.T.);
#1683=FACE_OUTER_BOUND('',#2398,.T.);
#1684=FACE_OUTER_BOUND('',#2399,.T.);
#1685=FACE_OUTER_BOUND('',#2400,.T.);
#1686=FACE_OUTER_BOUND('',#2401,.T.);
#1687=FACE_OUTER_BOUND('',#2402,.T.);
#1688=FACE_OUTER_BOUND('',#2403,.T.);
#1689=FACE_OUTER_BOUND('',#2404,.T.);
#1690=FACE_OUTER_BOUND('',#2405,.T.);
#1691=FACE_OUTER_BOUND('',#2406,.T.);
#1692=FACE_OUTER_BOUND('',#2407,.T.);
#1693=FACE_OUTER_BOUND('',#2408,.T.);
#1694=FACE_OUTER_BOUND('',#2409,.T.);
#1695=FACE_OUTER_BOUND('',#2410,.T.);
#1696=FACE_OUTER_BOUND('',#2411,.T.);
#1697=FACE_OUTER_BOUND('',#2412,.T.);
#1698=FACE_OUTER_BOUND('',#2413,.T.);
#1699=FACE_OUTER_BOUND('',#2414,.T.);
#1700=FACE_OUTER_BOUND('',#2416,.T.);
#1701=FACE_OUTER_BOUND('',#2417,.T.);
#1702=FACE_OUTER_BOUND('',#2418,.T.);
#1703=FACE_OUTER_BOUND('',#2419,.T.);
#1704=FACE_OUTER_BOUND('',#2420,.T.);
#1705=FACE_OUTER_BOUND('',#2422,.T.);
#1706=FACE_OUTER_BOUND('',#2423,.T.);
#1707=FACE_OUTER_BOUND('',#2425,.T.);
#1708=FACE_OUTER_BOUND('',#2426,.T.);
#1709=FACE_OUTER_BOUND('',#2427,.T.);
#1710=FACE_OUTER_BOUND('',#2428,.T.);
#1711=FACE_OUTER_BOUND('',#2429,.T.);
#1712=FACE_OUTER_BOUND('',#2431,.T.);
#1713=FACE_OUTER_BOUND('',#2432,.T.);
#1714=FACE_OUTER_BOUND('',#2433,.T.);
#1715=FACE_OUTER_BOUND('',#2434,.T.);
#1716=FACE_OUTER_BOUND('',#2435,.T.);
#1717=FACE_OUTER_BOUND('',#2436,.T.);
#1718=FACE_OUTER_BOUND('',#2437,.T.);
#1719=FACE_OUTER_BOUND('',#2438,.T.);
#1720=FACE_OUTER_BOUND('',#2439,.T.);
#1721=FACE_OUTER_BOUND('',#2440,.T.);
#1722=FACE_OUTER_BOUND('',#2441,.T.);
#1723=FACE_OUTER_BOUND('',#2442,.T.);
#1724=FACE_OUTER_BOUND('',#2443,.T.);
#1725=FACE_OUTER_BOUND('',#2444,.T.);
#1726=FACE_OUTER_BOUND('',#2445,.T.);
#1727=FACE_OUTER_BOUND('',#2446,.T.);
#1728=FACE_OUTER_BOUND('',#2447,.T.);
#1729=FACE_OUTER_BOUND('',#2448,.T.);
#1730=FACE_OUTER_BOUND('',#2449,.T.);
#1731=FACE_OUTER_BOUND('',#2450,.T.);
#1732=FACE_OUTER_BOUND('',#2451,.T.);
#1733=FACE_OUTER_BOUND('',#2452,.T.);
#1734=FACE_OUTER_BOUND('',#2453,.T.);
#1735=FACE_OUTER_BOUND('',#2454,.T.);
#1736=FACE_OUTER_BOUND('',#2455,.T.);
#1737=FACE_OUTER_BOUND('',#2456,.T.);
#1738=FACE_OUTER_BOUND('',#2458,.T.);
#1739=FACE_OUTER_BOUND('',#2459,.T.);
#1740=EDGE_LOOP('',(#5996,#5997,#5998,#5999));
#1741=EDGE_LOOP('',(#6000,#6001,#6002,#6003));
#1742=EDGE_LOOP('',(#6004,#6005,#6006,#6007));
#1743=EDGE_LOOP('',(#6008,#6009,#6010,#6011));
#1744=EDGE_LOOP('',(#6012,#6013,#6014,#6015));
#1745=EDGE_LOOP('',(#6016,#6017,#6018,#6019));
#1746=EDGE_LOOP('',(#6020,#6021,#6022,#6023));
#1747=EDGE_LOOP('',(#6024,#6025,#6026,#6027));
#1748=EDGE_LOOP('',(#6028,#6029,#6030,#6031));
#1749=EDGE_LOOP('',(#6032,#6033,#6034,#6035));
#1750=EDGE_LOOP('',(#6036,#6037,#6038,#6039));
#1751=EDGE_LOOP('',(#6040,#6041,#6042,#6043));
#1752=EDGE_LOOP('',(#6044,#6045,#6046,#6047));
#1753=EDGE_LOOP('',(#6048,#6049,#6050,#6051));
#1754=EDGE_LOOP('',(#6052,#6053,#6054,#6055));
#1755=EDGE_LOOP('',(#6056,#6057,#6058,#6059));
#1756=EDGE_LOOP('',(#6060,#6061,#6062,#6063));
#1757=EDGE_LOOP('',(#6064));
#1758=EDGE_LOOP('',(#6065));
#1759=EDGE_LOOP('',(#6066));
#1760=EDGE_LOOP('',(#6067));
#1761=EDGE_LOOP('',(#6068));
#1762=EDGE_LOOP('',(#6069));
#1763=EDGE_LOOP('',(#6070));
#1764=EDGE_LOOP('',(#6071));
#1765=EDGE_LOOP('',(#6072));
#1766=EDGE_LOOP('',(#6073));
#1767=EDGE_LOOP('',(#6074));
#1768=EDGE_LOOP('',(#6075));
#1769=EDGE_LOOP('',(#6076,#6077,#6078,#6079));
#1770=EDGE_LOOP('',(#6080));
#1771=EDGE_LOOP('',(#6081));
#1772=EDGE_LOOP('',(#6082));
#1773=EDGE_LOOP('',(#6083));
#1774=EDGE_LOOP('',(#6084));
#1775=EDGE_LOOP('',(#6085));
#1776=EDGE_LOOP('',(#6086));
#1777=EDGE_LOOP('',(#6087));
#1778=EDGE_LOOP('',(#6088));
#1779=EDGE_LOOP('',(#6089));
#1780=EDGE_LOOP('',(#6090));
#1781=EDGE_LOOP('',(#6091));
#1782=EDGE_LOOP('',(#6092,#6093,#6094,#6095));
#1783=EDGE_LOOP('',(#6096));
#1784=EDGE_LOOP('',(#6097,#6098,#6099,#6100));
#1785=EDGE_LOOP('',(#6101));
#1786=EDGE_LOOP('',(#6102,#6103,#6104,#6105));
#1787=EDGE_LOOP('',(#6106));
#1788=EDGE_LOOP('',(#6107));
#1789=EDGE_LOOP('',(#6108,#6109,#6110,#6111));
#1790=EDGE_LOOP('',(#6112));
#1791=EDGE_LOOP('',(#6113));
#1792=EDGE_LOOP('',(#6114,#6115,#6116,#6117));
#1793=EDGE_LOOP('',(#6118));
#1794=EDGE_LOOP('',(#6119));
#1795=EDGE_LOOP('',(#6120,#6121,#6122,#6123));
#1796=EDGE_LOOP('',(#6124));
#1797=EDGE_LOOP('',(#6125));
#1798=EDGE_LOOP('',(#6126,#6127,#6128,#6129));
#1799=EDGE_LOOP('',(#6130,#6131,#6132,#6133));
#1800=EDGE_LOOP('',(#6134,#6135,#6136,#6137));
#1801=EDGE_LOOP('',(#6138,#6139,#6140,#6141));
#1802=EDGE_LOOP('',(#6142,#6143,#6144,#6145));
#1803=EDGE_LOOP('',(#6146,#6147,#6148,#6149));
#1804=EDGE_LOOP('',(#6150,#6151,#6152,#6153));
#1805=EDGE_LOOP('',(#6154,#6155,#6156,#6157));
#1806=EDGE_LOOP('',(#6158,#6159,#6160,#6161));
#1807=EDGE_LOOP('',(#6162));
#1808=EDGE_LOOP('',(#6163));
#1809=EDGE_LOOP('',(#6164));
#1810=EDGE_LOOP('',(#6165));
#1811=EDGE_LOOP('',(#6166));
#1812=EDGE_LOOP('',(#6167));
#1813=EDGE_LOOP('',(#6168,#6169,#6170,#6171));
#1814=EDGE_LOOP('',(#6172));
#1815=EDGE_LOOP('',(#6173));
#1816=EDGE_LOOP('',(#6174));
#1817=EDGE_LOOP('',(#6175));
#1818=EDGE_LOOP('',(#6176,#6177,#6178,#6179));
#1819=EDGE_LOOP('',(#6180,#6181,#6182,#6183));
#1820=EDGE_LOOP('',(#6184));
#1821=EDGE_LOOP('',(#6185));
#1822=EDGE_LOOP('',(#6186));
#1823=EDGE_LOOP('',(#6187));
#1824=EDGE_LOOP('',(#6188,#6189,#6190,#6191));
#1825=EDGE_LOOP('',(#6192,#6193,#6194,#6195));
#1826=EDGE_LOOP('',(#6196));
#1827=EDGE_LOOP('',(#6197));
#1828=EDGE_LOOP('',(#6198));
#1829=EDGE_LOOP('',(#6199));
#1830=EDGE_LOOP('',(#6200,#6201,#6202,#6203));
#1831=EDGE_LOOP('',(#6204));
#1832=EDGE_LOOP('',(#6205,#6206,#6207,#6208));
#1833=EDGE_LOOP('',(#6209));
#1834=EDGE_LOOP('',(#6210,#6211,#6212,#6213));
#1835=EDGE_LOOP('',(#6214));
#1836=EDGE_LOOP('',(#6215));
#1837=EDGE_LOOP('',(#6216,#6217,#6218,#6219));
#1838=EDGE_LOOP('',(#6220));
#1839=EDGE_LOOP('',(#6221));
#1840=EDGE_LOOP('',(#6222,#6223,#6224,#6225));
#1841=EDGE_LOOP('',(#6226));
#1842=EDGE_LOOP('',(#6227));
#1843=EDGE_LOOP('',(#6228,#6229,#6230,#6231));
#1844=EDGE_LOOP('',(#6232));
#1845=EDGE_LOOP('',(#6233));
#1846=EDGE_LOOP('',(#6234,#6235,#6236,#6237));
#1847=EDGE_LOOP('',(#6238,#6239,#6240,#6241));
#1848=EDGE_LOOP('',(#6242,#6243,#6244,#6245));
#1849=EDGE_LOOP('',(#6246,#6247,#6248,#6249));
#1850=EDGE_LOOP('',(#6250,#6251,#6252,#6253));
#1851=EDGE_LOOP('',(#6254,#6255,#6256,#6257));
#1852=EDGE_LOOP('',(#6258,#6259,#6260,#6261));
#1853=EDGE_LOOP('',(#6262,#6263,#6264,#6265));
#1854=EDGE_LOOP('',(#6266,#6267,#6268,#6269));
#1855=EDGE_LOOP('',(#6270));
#1856=EDGE_LOOP('',(#6271));
#1857=EDGE_LOOP('',(#6272));
#1858=EDGE_LOOP('',(#6273));
#1859=EDGE_LOOP('',(#6274));
#1860=EDGE_LOOP('',(#6275));
#1861=EDGE_LOOP('',(#6276,#6277,#6278,#6279));
#1862=EDGE_LOOP('',(#6280));
#1863=EDGE_LOOP('',(#6281));
#1864=EDGE_LOOP('',(#6282));
#1865=EDGE_LOOP('',(#6283));
#1866=EDGE_LOOP('',(#6284,#6285,#6286,#6287));
#1867=EDGE_LOOP('',(#6288,#6289,#6290,#6291));
#1868=EDGE_LOOP('',(#6292));
#1869=EDGE_LOOP('',(#6293));
#1870=EDGE_LOOP('',(#6294));
#1871=EDGE_LOOP('',(#6295));
#1872=EDGE_LOOP('',(#6296,#6297,#6298,#6299));
#1873=EDGE_LOOP('',(#6300,#6301,#6302,#6303));
#1874=EDGE_LOOP('',(#6304));
#1875=EDGE_LOOP('',(#6305));
#1876=EDGE_LOOP('',(#6306));
#1877=EDGE_LOOP('',(#6307));
#1878=EDGE_LOOP('',(#6308,#6309,#6310,#6311));
#1879=EDGE_LOOP('',(#6312));
#1880=EDGE_LOOP('',(#6313,#6314,#6315,#6316));
#1881=EDGE_LOOP('',(#6317));
#1882=EDGE_LOOP('',(#6318,#6319,#6320,#6321));
#1883=EDGE_LOOP('',(#6322));
#1884=EDGE_LOOP('',(#6323,#6324,#6325,#6326));
#1885=EDGE_LOOP('',(#6327));
#1886=EDGE_LOOP('',(#6328,#6329,#6330,#6331));
#1887=EDGE_LOOP('',(#6332));
#1888=EDGE_LOOP('',(#6333));
#1889=EDGE_LOOP('',(#6334,#6335,#6336,#6337));
#1890=EDGE_LOOP('',(#6338));
#1891=EDGE_LOOP('',(#6339));
#1892=EDGE_LOOP('',(#6340,#6341,#6342,#6343));
#1893=EDGE_LOOP('',(#6344));
#1894=EDGE_LOOP('',(#6345));
#1895=EDGE_LOOP('',(#6346,#6347,#6348,#6349));
#1896=EDGE_LOOP('',(#6350));
#1897=EDGE_LOOP('',(#6351));
#1898=EDGE_LOOP('',(#6352,#6353,#6354,#6355));
#1899=EDGE_LOOP('',(#6356,#6357,#6358,#6359));
#1900=EDGE_LOOP('',(#6360,#6361,#6362,#6363));
#1901=EDGE_LOOP('',(#6364,#6365,#6366,#6367));
#1902=EDGE_LOOP('',(#6368,#6369,#6370,#6371));
#1903=EDGE_LOOP('',(#6372,#6373,#6374,#6375));
#1904=EDGE_LOOP('',(#6376,#6377,#6378,#6379));
#1905=EDGE_LOOP('',(#6380,#6381,#6382,#6383));
#1906=EDGE_LOOP('',(#6384,#6385,#6386,#6387));
#1907=EDGE_LOOP('',(#6388));
#1908=EDGE_LOOP('',(#6389));
#1909=EDGE_LOOP('',(#6390));
#1910=EDGE_LOOP('',(#6391));
#1911=EDGE_LOOP('',(#6392));
#1912=EDGE_LOOP('',(#6393));
#1913=EDGE_LOOP('',(#6394));
#1914=EDGE_LOOP('',(#6395));
#1915=EDGE_LOOP('',(#6396,#6397,#6398,#6399));
#1916=EDGE_LOOP('',(#6400));
#1917=EDGE_LOOP('',(#6401));
#1918=EDGE_LOOP('',(#6402));
#1919=EDGE_LOOP('',(#6403));
#1920=EDGE_LOOP('',(#6404,#6405,#6406,#6407));
#1921=EDGE_LOOP('',(#6408,#6409,#6410,#6411));
#1922=EDGE_LOOP('',(#6412,#6413,#6414,#6415));
#1923=EDGE_LOOP('',(#6416,#6417,#6418,#6419));
#1924=EDGE_LOOP('',(#6420,#6421,#6422,#6423));
#1925=EDGE_LOOP('',(#6424,#6425,#6426,#6427));
#1926=EDGE_LOOP('',(#6428,#6429,#6430,#6431));
#1927=EDGE_LOOP('',(#6432,#6433,#6434,#6435));
#1928=EDGE_LOOP('',(#6436,#6437,#6438,#6439));
#1929=EDGE_LOOP('',(#6440,#6441,#6442,#6443));
#1930=EDGE_LOOP('',(#6444,#6445,#6446,#6447));
#1931=EDGE_LOOP('',(#6448,#6449,#6450,#6451));
#1932=EDGE_LOOP('',(#6452,#6453,#6454,#6455));
#1933=EDGE_LOOP('',(#6456,#6457,#6458,#6459));
#1934=EDGE_LOOP('',(#6460,#6461));
#1935=EDGE_LOOP('',(#6462));
#1936=EDGE_LOOP('',(#6463));
#1937=EDGE_LOOP('',(#6464,#6465,#6466));
#1938=EDGE_LOOP('',(#6467,#6468,#6469));
#1939=EDGE_LOOP('',(#6470,#6471,#6472));
#1940=EDGE_LOOP('',(#6473,#6474,#6475,#6476));
#1941=EDGE_LOOP('',(#6477,#6478,#6479));
#1942=EDGE_LOOP('',(#6480,#6481,#6482,#6483));
#1943=EDGE_LOOP('',(#6484,#6485,#6486,#6487));
#1944=EDGE_LOOP('',(#6488));
#1945=EDGE_LOOP('',(#6489));
#1946=EDGE_LOOP('',(#6490,#6491,#6492,#6493,#6494,#6495,#6496,#6497,#6498,
#6499,#6500,#6501));
#1947=EDGE_LOOP('',(#6502,#6503,#6504,#6505,#6506,#6507,#6508,#6509,#6510,
#6511,#6512,#6513));
#1948=EDGE_LOOP('',(#6514,#6515));
#1949=EDGE_LOOP('',(#6516));
#1950=EDGE_LOOP('',(#6517,#6518));
#1951=EDGE_LOOP('',(#6519));
#1952=EDGE_LOOP('',(#6520,#6521,#6522,#6523));
#1953=EDGE_LOOP('',(#6524,#6525,#6526,#6527));
#1954=EDGE_LOOP('',(#6528,#6529,#6530,#6531));
#1955=EDGE_LOOP('',(#6532,#6533,#6534,#6535));
#1956=EDGE_LOOP('',(#6536,#6537,#6538,#6539));
#1957=EDGE_LOOP('',(#6540,#6541,#6542,#6543));
#1958=EDGE_LOOP('',(#6544,#6545,#6546,#6547));
#1959=EDGE_LOOP('',(#6548,#6549,#6550,#6551));
#1960=EDGE_LOOP('',(#6552,#6553,#6554,#6555));
#1961=EDGE_LOOP('',(#6556,#6557,#6558,#6559));
#1962=EDGE_LOOP('',(#6560,#6561,#6562,#6563));
#1963=EDGE_LOOP('',(#6564,#6565,#6566,#6567));
#1964=EDGE_LOOP('',(#6568,#6569,#6570,#6571));
#1965=EDGE_LOOP('',(#6572));
#1966=EDGE_LOOP('',(#6573));
#1967=EDGE_LOOP('',(#6574,#6575,#6576,#6577));
#1968=EDGE_LOOP('',(#6578));
#1969=EDGE_LOOP('',(#6579));
#1970=EDGE_LOOP('',(#6580,#6581));
#1971=EDGE_LOOP('',(#6582));
#1972=EDGE_LOOP('',(#6583));
#1973=EDGE_LOOP('',(#6584));
#1974=EDGE_LOOP('',(#6585));
#1975=EDGE_LOOP('',(#6586,#6587,#6588,#6589,#6590,#6591));
#1976=EDGE_LOOP('',(#6592,#6593,#6594,#6595,#6596,#6597));
#1977=EDGE_LOOP('',(#6598,#6599,#6600,#6601));
#1978=EDGE_LOOP('',(#6602,#6603,#6604));
#1979=EDGE_LOOP('',(#6605,#6606,#6607));
#1980=EDGE_LOOP('',(#6608,#6609,#6610));
#1981=EDGE_LOOP('',(#6611,#6612,#6613));
#1982=EDGE_LOOP('',(#6614,#6615,#6616));
#1983=EDGE_LOOP('',(#6617,#6618,#6619));
#1984=EDGE_LOOP('',(#6620,#6621,#6622,#6623,#6624,#6625));
#1985=EDGE_LOOP('',(#6626,#6627,#6628,#6629,#6630,#6631));
#1986=EDGE_LOOP('',(#6632,#6633,#6634,#6635,#6636,#6637));
#1987=EDGE_LOOP('',(#6638,#6639,#6640,#6641,#6642,#6643));
#1988=EDGE_LOOP('',(#6644));
#1989=EDGE_LOOP('',(#6645));
#1990=EDGE_LOOP('',(#6646));
#1991=EDGE_LOOP('',(#6647));
#1992=EDGE_LOOP('',(#6648,#6649,#6650,#6651));
#1993=EDGE_LOOP('',(#6652));
#1994=EDGE_LOOP('',(#6653));
#1995=EDGE_LOOP('',(#6654,#6655,#6656,#6657));
#1996=EDGE_LOOP('',(#6658));
#1997=EDGE_LOOP('',(#6659));
#1998=EDGE_LOOP('',(#6660));
#1999=EDGE_LOOP('',(#6661));
#2000=EDGE_LOOP('',(#6662));
#2001=EDGE_LOOP('',(#6663));
#2002=EDGE_LOOP('',(#6664,#6665,#6666,#6667));
#2003=EDGE_LOOP('',(#6668,#6669,#6670,#6671));
#2004=EDGE_LOOP('',(#6672));
#2005=EDGE_LOOP('',(#6673));
#2006=EDGE_LOOP('',(#6674));
#2007=EDGE_LOOP('',(#6675));
#2008=EDGE_LOOP('',(#6676,#6677,#6678,#6679));
#2009=EDGE_LOOP('',(#6680,#6681,#6682,#6683));
#2010=EDGE_LOOP('',(#6684,#6685,#6686,#6687));
#2011=EDGE_LOOP('',(#6688,#6689,#6690,#6691));
#2012=EDGE_LOOP('',(#6692,#6693,#6694,#6695));
#2013=EDGE_LOOP('',(#6696,#6697,#6698,#6699));
#2014=EDGE_LOOP('',(#6700,#6701,#6702,#6703,#6704,#6705));
#2015=EDGE_LOOP('',(#6706,#6707,#6708,#6709,#6710,#6711));
#2016=EDGE_LOOP('',(#6712));
#2017=EDGE_LOOP('',(#6713));
#2018=EDGE_LOOP('',(#6714,#6715,#6716,#6717));
#2019=EDGE_LOOP('',(#6718,#6719,#6720,#6721));
#2020=EDGE_LOOP('',(#6722,#6723,#6724,#6725));
#2021=EDGE_LOOP('',(#6726));
#2022=EDGE_LOOP('',(#6727));
#2023=EDGE_LOOP('',(#6728,#6729,#6730,#6731));
#2024=EDGE_LOOP('',(#6732,#6733,#6734,#6735));
#2025=EDGE_LOOP('',(#6736,#6737,#6738,#6739));
#2026=EDGE_LOOP('',(#6740));
#2027=EDGE_LOOP('',(#6741));
#2028=EDGE_LOOP('',(#6742,#6743,#6744,#6745));
#2029=EDGE_LOOP('',(#6746));
#2030=EDGE_LOOP('',(#6747));
#2031=EDGE_LOOP('',(#6748,#6749,#6750,#6751));
#2032=EDGE_LOOP('',(#6752));
#2033=EDGE_LOOP('',(#6753));
#2034=EDGE_LOOP('',(#6754,#6755,#6756,#6757));
#2035=EDGE_LOOP('',(#6758));
#2036=EDGE_LOOP('',(#6759));
#2037=EDGE_LOOP('',(#6760,#6761,#6762,#6763));
#2038=EDGE_LOOP('',(#6764,#6765,#6766,#6767));
#2039=EDGE_LOOP('',(#6768,#6769,#6770,#6771));
#2040=EDGE_LOOP('',(#6772,#6773,#6774,#6775));
#2041=EDGE_LOOP('',(#6776,#6777,#6778,#6779));
#2042=EDGE_LOOP('',(#6780,#6781,#6782,#6783));
#2043=EDGE_LOOP('',(#6784,#6785,#6786,#6787));
#2044=EDGE_LOOP('',(#6788,#6789,#6790,#6791));
#2045=EDGE_LOOP('',(#6792,#6793,#6794,#6795));
#2046=EDGE_LOOP('',(#6796));
#2047=EDGE_LOOP('',(#6797));
#2048=EDGE_LOOP('',(#6798));
#2049=EDGE_LOOP('',(#6799));
#2050=EDGE_LOOP('',(#6800,#6801,#6802,#6803));
#2051=EDGE_LOOP('',(#6804,#6805,#6806,#6807));
#2052=EDGE_LOOP('',(#6808,#6809,#6810,#6811));
#2053=EDGE_LOOP('',(#6812,#6813,#6814,#6815));
#2054=EDGE_LOOP('',(#6816,#6817,#6818,#6819));
#2055=EDGE_LOOP('',(#6820,#6821,#6822,#6823));
#2056=EDGE_LOOP('',(#6824));
#2057=EDGE_LOOP('',(#6825));
#2058=EDGE_LOOP('',(#6826));
#2059=EDGE_LOOP('',(#6827));
#2060=EDGE_LOOP('',(#6828,#6829,#6830,#6831));
#2061=EDGE_LOOP('',(#6832,#6833,#6834,#6835,#6836,#6837,#6838,#6839,#6840,
#6841,#6842,#6843));
#2062=EDGE_LOOP('',(#6844,#6845,#6846,#6847,#6848,#6849,#6850,#6851,#6852,
#6853,#6854,#6855));
#2063=EDGE_LOOP('',(#6856));
#2064=EDGE_LOOP('',(#6857,#6858,#6859,#6860));
#2065=EDGE_LOOP('',(#6861,#6862,#6863,#6864));
#2066=EDGE_LOOP('',(#6865,#6866,#6867,#6868));
#2067=EDGE_LOOP('',(#6869));
#2068=EDGE_LOOP('',(#6870));
#2069=EDGE_LOOP('',(#6871,#6872,#6873,#6874));
#2070=EDGE_LOOP('',(#6875,#6876,#6877,#6878));
#2071=EDGE_LOOP('',(#6879,#6880,#6881,#6882));
#2072=EDGE_LOOP('',(#6883));
#2073=EDGE_LOOP('',(#6884,#6885,#6886,#6887));
#2074=EDGE_LOOP('',(#6888,#6889,#6890,#6891));
#2075=EDGE_LOOP('',(#6892,#6893,#6894,#6895));
#2076=EDGE_LOOP('',(#6896,#6897,#6898,#6899));
#2077=EDGE_LOOP('',(#6900,#6901,#6902,#6903));
#2078=EDGE_LOOP('',(#6904,#6905,#6906,#6907));
#2079=EDGE_LOOP('',(#6908,#6909,#6910,#6911,#6912,#6913));
#2080=EDGE_LOOP('',(#6914,#6915,#6916,#6917,#6918,#6919));
#2081=EDGE_LOOP('',(#6920,#6921,#6922,#6923));
#2082=EDGE_LOOP('',(#6924,#6925,#6926,#6927));
#2083=EDGE_LOOP('',(#6928,#6929,#6930,#6931));
#2084=EDGE_LOOP('',(#6932,#6933,#6934,#6935));
#2085=EDGE_LOOP('',(#6936,#6937,#6938,#6939,#6940,#6941,#6942,#6943));
#2086=EDGE_LOOP('',(#6944,#6945,#6946,#6947,#6948));
#2087=EDGE_LOOP('',(#6949));
#2088=EDGE_LOOP('',(#6950,#6951));
#2089=EDGE_LOOP('',(#6952,#6953,#6954,#6955,#6956,#6957,#6958,#6959,#6960));
#2090=EDGE_LOOP('',(#6961,#6962,#6963));
#2091=EDGE_LOOP('',(#6964,#6965,#6966,#6967));
#2092=EDGE_LOOP('',(#6968,#6969,#6970,#6971));
#2093=EDGE_LOOP('',(#6972,#6973,#6974,#6975));
#2094=EDGE_LOOP('',(#6976,#6977));
#2095=EDGE_LOOP('',(#6978));
#2096=EDGE_LOOP('',(#6979));
#2097=EDGE_LOOP('',(#6980));
#2098=EDGE_LOOP('',(#6981));
#2099=EDGE_LOOP('',(#6982,#6983));
#2100=EDGE_LOOP('',(#6984,#6985,#6986,#6987,#6988,#6989,#6990,#6991,#6992));
#2101=EDGE_LOOP('',(#6993,#6994,#6995));
#2102=EDGE_LOOP('',(#6996,#6997,#6998,#6999));
#2103=EDGE_LOOP('',(#7000,#7001,#7002,#7003));
#2104=EDGE_LOOP('',(#7004,#7005,#7006,#7007));
#2105=EDGE_LOOP('',(#7008,#7009));
#2106=EDGE_LOOP('',(#7010));
#2107=EDGE_LOOP('',(#7011));
#2108=EDGE_LOOP('',(#7012));
#2109=EDGE_LOOP('',(#7013));
#2110=EDGE_LOOP('',(#7014,#7015,#7016,#7017));
#2111=EDGE_LOOP('',(#7018,#7019,#7020,#7021));
#2112=EDGE_LOOP('',(#7022));
#2113=EDGE_LOOP('',(#7023));
#2114=EDGE_LOOP('',(#7024));
#2115=EDGE_LOOP('',(#7025));
#2116=EDGE_LOOP('',(#7026,#7027));
#2117=EDGE_LOOP('',(#7028,#7029,#7030,#7031,#7032,#7033,#7034,#7035));
#2118=EDGE_LOOP('',(#7036,#7037,#7038,#7039,#7040,#7041,#7042,#7043,#7044,
#7045,#7046,#7047,#7048,#7049));
#2119=EDGE_LOOP('',(#7050,#7051,#7052,#7053,#7054,#7055,#7056));
#2120=EDGE_LOOP('',(#7057));
#2121=EDGE_LOOP('',(#7058));
#2122=EDGE_LOOP('',(#7059,#7060,#7061,#7062));
#2123=EDGE_LOOP('',(#7063,#7064,#7065,#7066));
#2124=EDGE_LOOP('',(#7067,#7068));
#2125=EDGE_LOOP('',(#7069,#7070,#7071,#7072,#7073,#7074,#7075,#7076));
#2126=EDGE_LOOP('',(#7077,#7078));
#2127=EDGE_LOOP('',(#7079,#7080,#7081,#7082));
#2128=EDGE_LOOP('',(#7083));
#2129=EDGE_LOOP('',(#7084));
#2130=EDGE_LOOP('',(#7085,#7086,#7087,#7088));
#2131=EDGE_LOOP('',(#7089,#7090,#7091,#7092,#7093,#7094));
#2132=EDGE_LOOP('',(#7095,#7096,#7097,#7098,#7099,#7100,#7101,#7102,#7103));
#2133=EDGE_LOOP('',(#7104,#7105,#7106,#7107));
#2134=EDGE_LOOP('',(#7108));
#2135=EDGE_LOOP('',(#7109));
#2136=EDGE_LOOP('',(#7110));
#2137=EDGE_LOOP('',(#7111,#7112,#7113,#7114));
#2138=EDGE_LOOP('',(#7115));
#2139=EDGE_LOOP('',(#7116));
#2140=EDGE_LOOP('',(#7117,#7118,#7119,#7120));
#2141=EDGE_LOOP('',(#7121));
#2142=EDGE_LOOP('',(#7122,#7123,#7124,#7125));
#2143=EDGE_LOOP('',(#7126,#7127,#7128,#7129));
#2144=EDGE_LOOP('',(#7130));
#2145=EDGE_LOOP('',(#7131));
#2146=EDGE_LOOP('',(#7132));
#2147=EDGE_LOOP('',(#7133));
#2148=EDGE_LOOP('',(#7134,#7135,#7136,#7137));
#2149=EDGE_LOOP('',(#7138,#7139,#7140,#7141));
#2150=EDGE_LOOP('',(#7142));
#2151=EDGE_LOOP('',(#7143));
#2152=EDGE_LOOP('',(#7144));
#2153=EDGE_LOOP('',(#7145));
#2154=EDGE_LOOP('',(#7146,#7147,#7148,#7149));
#2155=EDGE_LOOP('',(#7150,#7151,#7152,#7153));
#2156=EDGE_LOOP('',(#7154));
#2157=EDGE_LOOP('',(#7155));
#2158=EDGE_LOOP('',(#7156));
#2159=EDGE_LOOP('',(#7157));
#2160=EDGE_LOOP('',(#7158,#7159,#7160,#7161,#7162,#7163,#7164,#7165));
#2161=EDGE_LOOP('',(#7166,#7167,#7168,#7169));
#2162=EDGE_LOOP('',(#7170,#7171,#7172,#7173));
#2163=EDGE_LOOP('',(#7174,#7175,#7176,#7177));
#2164=EDGE_LOOP('',(#7178,#7179,#7180,#7181));
#2165=EDGE_LOOP('',(#7182,#7183,#7184,#7185,#7186,#7187,#7188,#7189));
#2166=EDGE_LOOP('',(#7190,#7191,#7192,#7193));
#2167=EDGE_LOOP('',(#7194,#7195,#7196,#7197));
#2168=EDGE_LOOP('',(#7198,#7199,#7200,#7201));
#2169=EDGE_LOOP('',(#7202,#7203,#7204,#7205));
#2170=EDGE_LOOP('',(#7206,#7207,#7208,#7209));
#2171=EDGE_LOOP('',(#7210,#7211,#7212,#7213));
#2172=EDGE_LOOP('',(#7214,#7215,#7216,#7217));
#2173=EDGE_LOOP('',(#7218,#7219,#7220,#7221));
#2174=EDGE_LOOP('',(#7222,#7223,#7224,#7225));
#2175=EDGE_LOOP('',(#7226,#7227,#7228,#7229));
#2176=EDGE_LOOP('',(#7230,#7231,#7232,#7233,#7234,#7235));
#2177=EDGE_LOOP('',(#7236));
#2178=EDGE_LOOP('',(#7237,#7238,#7239,#7240,#7241,#7242));
#2179=EDGE_LOOP('',(#7243,#7244,#7245,#7246));
#2180=EDGE_LOOP('',(#7247,#7248,#7249,#7250));
#2181=EDGE_LOOP('',(#7251,#7252,#7253,#7254));
#2182=EDGE_LOOP('',(#7255));
#2183=EDGE_LOOP('',(#7256,#7257,#7258,#7259));
#2184=EDGE_LOOP('',(#7260,#7261,#7262,#7263));
#2185=EDGE_LOOP('',(#7264,#7265,#7266,#7267));
#2186=EDGE_LOOP('',(#7268,#7269,#7270,#7271));
#2187=EDGE_LOOP('',(#7272));
#2188=EDGE_LOOP('',(#7273));
#2189=EDGE_LOOP('',(#7274,#7275,#7276,#7277));
#2190=EDGE_LOOP('',(#7278,#7279,#7280,#7281));
#2191=EDGE_LOOP('',(#7282,#7283,#7284,#7285));
#2192=EDGE_LOOP('',(#7286,#7287,#7288,#7289));
#2193=EDGE_LOOP('',(#7290));
#2194=EDGE_LOOP('',(#7291));
#2195=EDGE_LOOP('',(#7292,#7293,#7294,#7295));
#2196=EDGE_LOOP('',(#7296,#7297,#7298,#7299));
#2197=EDGE_LOOP('',(#7300));
#2198=EDGE_LOOP('',(#7301));
#2199=EDGE_LOOP('',(#7302));
#2200=EDGE_LOOP('',(#7303));
#2201=EDGE_LOOP('',(#7304,#7305,#7306,#7307));
#2202=EDGE_LOOP('',(#7308,#7309,#7310,#7311));
#2203=EDGE_LOOP('',(#7312));
#2204=EDGE_LOOP('',(#7313));
#2205=EDGE_LOOP('',(#7314));
#2206=EDGE_LOOP('',(#7315));
#2207=EDGE_LOOP('',(#7316,#7317,#7318,#7319));
#2208=EDGE_LOOP('',(#7320,#7321,#7322,#7323));
#2209=EDGE_LOOP('',(#7324));
#2210=EDGE_LOOP('',(#7325));
#2211=EDGE_LOOP('',(#7326));
#2212=EDGE_LOOP('',(#7327));
#2213=EDGE_LOOP('',(#7328,#7329,#7330,#7331));
#2214=EDGE_LOOP('',(#7332,#7333,#7334,#7335));
#2215=EDGE_LOOP('',(#7336));
#2216=EDGE_LOOP('',(#7337));
#2217=EDGE_LOOP('',(#7338));
#2218=EDGE_LOOP('',(#7339));
#2219=EDGE_LOOP('',(#7340,#7341,#7342,#7343,#7344,#7345));
#2220=EDGE_LOOP('',(#7346,#7347,#7348,#7349,#7350));
#2221=EDGE_LOOP('',(#7351,#7352,#7353,#7354));
#2222=EDGE_LOOP('',(#7355,#7356,#7357,#7358));
#2223=EDGE_LOOP('',(#7359));
#2224=EDGE_LOOP('',(#7360));
#2225=EDGE_LOOP('',(#7361,#7362,#7363,#7364,#7365));
#2226=EDGE_LOOP('',(#7366));
#2227=EDGE_LOOP('',(#7367));
#2228=EDGE_LOOP('',(#7368,#7369,#7370,#7371));
#2229=EDGE_LOOP('',(#7372,#7373,#7374,#7375,#7376,#7377));
#2230=EDGE_LOOP('',(#7378,#7379,#7380,#7381,#7382));
#2231=EDGE_LOOP('',(#7383));
#2232=EDGE_LOOP('',(#7384));
#2233=EDGE_LOOP('',(#7385,#7386,#7387,#7388));
#2234=EDGE_LOOP('',(#7389,#7390,#7391,#7392));
#2235=EDGE_LOOP('',(#7393,#7394,#7395,#7396));
#2236=EDGE_LOOP('',(#7397));
#2237=EDGE_LOOP('',(#7398));
#2238=EDGE_LOOP('',(#7399,#7400,#7401,#7402,#7403));
#2239=EDGE_LOOP('',(#7404,#7405));
#2240=EDGE_LOOP('',(#7406,#7407));
#2241=EDGE_LOOP('',(#7408,#7409));
#2242=EDGE_LOOP('',(#7410,#7411));
#2243=EDGE_LOOP('',(#7412,#7413));
#2244=EDGE_LOOP('',(#7414,#7415));
#2245=EDGE_LOOP('',(#7416,#7417));
#2246=EDGE_LOOP('',(#7418,#7419));
#2247=EDGE_LOOP('',(#7420,#7421,#7422,#7423));
#2248=EDGE_LOOP('',(#7424,#7425,#7426,#7427,#7428,#7429,#7430,#7431,#7432,
#7433,#7434,#7435,#7436,#7437,#7438,#7439,#7440,#7441,#7442,#7443));
#2249=EDGE_LOOP('',(#7444,#7445,#7446,#7447));
#2250=EDGE_LOOP('',(#7448,#7449,#7450,#7451));
#2251=EDGE_LOOP('',(#7452,#7453,#7454,#7455));
#2252=EDGE_LOOP('',(#7456,#7457,#7458,#7459));
#2253=EDGE_LOOP('',(#7460,#7461,#7462,#7463));
#2254=EDGE_LOOP('',(#7464,#7465,#7466,#7467,#7468,#7469));
#2255=EDGE_LOOP('',(#7470,#7471,#7472,#7473));
#2256=EDGE_LOOP('',(#7474,#7475,#7476,#7477));
#2257=EDGE_LOOP('',(#7478,#7479,#7480,#7481));
#2258=EDGE_LOOP('',(#7482,#7483,#7484,#7485));
#2259=EDGE_LOOP('',(#7486,#7487,#7488,#7489));
#2260=EDGE_LOOP('',(#7490,#7491,#7492,#7493));
#2261=EDGE_LOOP('',(#7494,#7495,#7496,#7497,#7498,#7499,#7500,#7501,#7502,
#7503,#7504,#7505,#7506,#7507,#7508,#7509,#7510,#7511,#7512,#7513));
#2262=EDGE_LOOP('',(#7514,#7515,#7516,#7517));
#2263=EDGE_LOOP('',(#7518,#7519,#7520,#7521));
#2264=EDGE_LOOP('',(#7522));
#2265=EDGE_LOOP('',(#7523));
#2266=EDGE_LOOP('',(#7524,#7525,#7526,#7527));
#2267=EDGE_LOOP('',(#7528));
#2268=EDGE_LOOP('',(#7529));
#2269=EDGE_LOOP('',(#7530,#7531,#7532,#7533));
#2270=EDGE_LOOP('',(#7534));
#2271=EDGE_LOOP('',(#7535));
#2272=EDGE_LOOP('',(#7536,#7537,#7538,#7539));
#2273=EDGE_LOOP('',(#7540));
#2274=EDGE_LOOP('',(#7541));
#2275=EDGE_LOOP('',(#7542,#7543,#7544,#7545));
#2276=EDGE_LOOP('',(#7546));
#2277=EDGE_LOOP('',(#7547));
#2278=EDGE_LOOP('',(#7548,#7549,#7550,#7551));
#2279=EDGE_LOOP('',(#7552,#7553,#7554,#7555));
#2280=EDGE_LOOP('',(#7556));
#2281=EDGE_LOOP('',(#7557,#7558,#7559,#7560));
#2282=EDGE_LOOP('',(#7561));
#2283=EDGE_LOOP('',(#7562,#7563,#7564,#7565));
#2284=EDGE_LOOP('',(#7566,#7567,#7568,#7569));
#2285=EDGE_LOOP('',(#7570,#7571,#7572,#7573));
#2286=EDGE_LOOP('',(#7574));
#2287=EDGE_LOOP('',(#7575));
#2288=EDGE_LOOP('',(#7576,#7577,#7578,#7579));
#2289=EDGE_LOOP('',(#7580,#7581,#7582,#7583));
#2290=EDGE_LOOP('',(#7584,#7585,#7586,#7587));
#2291=EDGE_LOOP('',(#7588));
#2292=EDGE_LOOP('',(#7589,#7590,#7591,#7592));
#2293=EDGE_LOOP('',(#7593,#7594,#7595,#7596));
#2294=EDGE_LOOP('',(#7597,#7598,#7599,#7600));
#2295=EDGE_LOOP('',(#7601,#7602,#7603,#7604));
#2296=EDGE_LOOP('',(#7605));
#2297=EDGE_LOOP('',(#7606,#7607,#7608,#7609));
#2298=EDGE_LOOP('',(#7610,#7611,#7612,#7613));
#2299=EDGE_LOOP('',(#7614,#7615,#7616,#7617));
#2300=EDGE_LOOP('',(#7618,#7619,#7620,#7621));
#2301=EDGE_LOOP('',(#7622,#7623,#7624,#7625));
#2302=EDGE_LOOP('',(#7626,#7627,#7628,#7629));
#2303=EDGE_LOOP('',(#7630,#7631,#7632,#7633,#7634,#7635,#7636,#7637));
#2304=EDGE_LOOP('',(#7638,#7639,#7640,#7641));
#2305=EDGE_LOOP('',(#7642,#7643,#7644,#7645,#7646,#7647,#7648,#7649));
#2306=EDGE_LOOP('',(#7650,#7651,#7652,#7653));
#2307=EDGE_LOOP('',(#7654));
#2308=EDGE_LOOP('',(#7655));
#2309=EDGE_LOOP('',(#7656));
#2310=EDGE_LOOP('',(#7657));
#2311=EDGE_LOOP('',(#7658,#7659,#7660,#7661));
#2312=EDGE_LOOP('',(#7662));
#2313=EDGE_LOOP('',(#7663));
#2314=EDGE_LOOP('',(#7664));
#2315=EDGE_LOOP('',(#7665));
#2316=EDGE_LOOP('',(#7666,#7667,#7668,#7669));
#2317=EDGE_LOOP('',(#7670,#7671,#7672,#7673));
#2318=EDGE_LOOP('',(#7674,#7675,#7676,#7677));
#2319=EDGE_LOOP('',(#7678,#7679,#7680,#7681));
#2320=EDGE_LOOP('',(#7682,#7683,#7684,#7685));
#2321=EDGE_LOOP('',(#7686,#7687,#7688,#7689));
#2322=EDGE_LOOP('',(#7690,#7691,#7692,#7693));
#2323=EDGE_LOOP('',(#7694));
#2324=EDGE_LOOP('',(#7695));
#2325=EDGE_LOOP('',(#7696,#7697,#7698,#7699));
#2326=EDGE_LOOP('',(#7700));
#2327=EDGE_LOOP('',(#7701));
#2328=EDGE_LOOP('',(#7702,#7703,#7704,#7705));
#2329=EDGE_LOOP('',(#7706));
#2330=EDGE_LOOP('',(#7707));
#2331=EDGE_LOOP('',(#7708));
#2332=EDGE_LOOP('',(#7709,#7710,#7711,#7712));
#2333=EDGE_LOOP('',(#7713));
#2334=EDGE_LOOP('',(#7714,#7715,#7716,#7717));
#2335=EDGE_LOOP('',(#7718));
#2336=EDGE_LOOP('',(#7719));
#2337=EDGE_LOOP('',(#7720,#7721,#7722,#7723));
#2338=EDGE_LOOP('',(#7724,#7725,#7726,#7727));
#2339=EDGE_LOOP('',(#7728));
#2340=EDGE_LOOP('',(#7729));
#2341=EDGE_LOOP('',(#7730));
#2342=EDGE_LOOP('',(#7731));
#2343=EDGE_LOOP('',(#7732,#7733,#7734,#7735));
#2344=EDGE_LOOP('',(#7736,#7737,#7738,#7739));
#2345=EDGE_LOOP('',(#7740));
#2346=EDGE_LOOP('',(#7741));
#2347=EDGE_LOOP('',(#7742));
#2348=EDGE_LOOP('',(#7743));
#2349=EDGE_LOOP('',(#7744,#7745,#7746,#7747));
#2350=EDGE_LOOP('',(#7748,#7749,#7750,#7751));
#2351=EDGE_LOOP('',(#7752));
#2352=EDGE_LOOP('',(#7753));
#2353=EDGE_LOOP('',(#7754));
#2354=EDGE_LOOP('',(#7755));
#2355=EDGE_LOOP('',(#7756,#7757));
#2356=EDGE_LOOP('',(#7758,#7759,#7760,#7761,#7762,#7763,#7764,#7765));
#2357=EDGE_LOOP('',(#7766,#7767));
#2358=EDGE_LOOP('',(#7768,#7769,#7770,#7771,#7772,#7773,#7774,#7775));
#2359=EDGE_LOOP('',(#7776,#7777));
#2360=EDGE_LOOP('',(#7778,#7779,#7780,#7781,#7782,#7783,#7784,#7785));
#2361=EDGE_LOOP('',(#7786,#7787));
#2362=EDGE_LOOP('',(#7788,#7789,#7790,#7791,#7792,#7793,#7794,#7795));
#2363=EDGE_LOOP('',(#7796,#7797,#7798,#7799,#7800,#7801,#7802,#7803,#7804,
#7805,#7806,#7807));
#2364=EDGE_LOOP('',(#7808,#7809,#7810,#7811,#7812,#7813,#7814,#7815,#7816,
#7817,#7818,#7819));
#2365=EDGE_LOOP('',(#7820,#7821,#7822,#7823,#7824,#7825,#7826,#7827,#7828,
#7829,#7830,#7831));
#2366=EDGE_LOOP('',(#7832,#7833,#7834,#7835,#7836,#7837,#7838,#7839,#7840,
#7841));
#2367=EDGE_LOOP('',(#7842,#7843,#7844,#7845));
#2368=EDGE_LOOP('',(#7846,#7847,#7848,#7849));
#2369=EDGE_LOOP('',(#7850));
#2370=EDGE_LOOP('',(#7851));
#2371=EDGE_LOOP('',(#7852));
#2372=EDGE_LOOP('',(#7853));
#2373=EDGE_LOOP('',(#7854,#7855,#7856,#7857));
#2374=EDGE_LOOP('',(#7858,#7859,#7860,#7861,#7862,#7863,#7864,#7865,#7866,
#7867));
#2375=EDGE_LOOP('',(#7868,#7869,#7870,#7871));
#2376=EDGE_LOOP('',(#7872,#7873,#7874,#7875));
#2377=EDGE_LOOP('',(#7876,#7877,#7878,#7879));
#2378=EDGE_LOOP('',(#7880,#7881,#7882,#7883));
#2379=EDGE_LOOP('',(#7884,#7885,#7886,#7887));
#2380=EDGE_LOOP('',(#7888,#7889,#7890,#7891,#7892,#7893,#7894,#7895,#7896,
#7897,#7898,#7899));
#2381=EDGE_LOOP('',(#7900,#7901,#7902,#7903));
#2382=EDGE_LOOP('',(#7904,#7905,#7906,#7907));
#2383=EDGE_LOOP('',(#7908,#7909,#7910,#7911));
#2384=EDGE_LOOP('',(#7912,#7913,#7914,#7915));
#2385=EDGE_LOOP('',(#7916,#7917,#7918,#7919));
#2386=EDGE_LOOP('',(#7920,#7921,#7922,#7923));
#2387=EDGE_LOOP('',(#7924,#7925,#7926,#7927));
#2388=EDGE_LOOP('',(#7928,#7929,#7930,#7931));
#2389=EDGE_LOOP('',(#7932,#7933,#7934,#7935,#7936,#7937,#7938,#7939));
#2390=EDGE_LOOP('',(#7940,#7941,#7942,#7943,#7944,#7945,#7946,#7947));
#2391=EDGE_LOOP('',(#7948,#7949,#7950,#7951));
#2392=EDGE_LOOP('',(#7952,#7953,#7954,#7955));
#2393=EDGE_LOOP('',(#7956,#7957,#7958,#7959));
#2394=EDGE_LOOP('',(#7960,#7961,#7962,#7963));
#2395=EDGE_LOOP('',(#7964,#7965,#7966,#7967));
#2396=EDGE_LOOP('',(#7968,#7969,#7970,#7971));
#2397=EDGE_LOOP('',(#7972,#7973,#7974,#7975));
#2398=EDGE_LOOP('',(#7976,#7977,#7978,#7979));
#2399=EDGE_LOOP('',(#7980,#7981,#7982,#7983,#7984,#7985,#7986,#7987));
#2400=EDGE_LOOP('',(#7988,#7989,#7990,#7991,#7992,#7993,#7994,#7995));
#2401=EDGE_LOOP('',(#7996,#7997,#7998,#7999));
#2402=EDGE_LOOP('',(#8000,#8001,#8002,#8003));
#2403=EDGE_LOOP('',(#8004,#8005,#8006,#8007));
#2404=EDGE_LOOP('',(#8008,#8009,#8010,#8011));
#2405=EDGE_LOOP('',(#8012,#8013,#8014,#8015));
#2406=EDGE_LOOP('',(#8016,#8017,#8018,#8019));
#2407=EDGE_LOOP('',(#8020,#8021,#8022,#8023,#8024,#8025));
#2408=EDGE_LOOP('',(#8026,#8027,#8028,#8029,#8030,#8031));
#2409=EDGE_LOOP('',(#8032));
#2410=EDGE_LOOP('',(#8033));
#2411=EDGE_LOOP('',(#8034,#8035,#8036,#8037));
#2412=EDGE_LOOP('',(#8038,#8039,#8040,#8041));
#2413=EDGE_LOOP('',(#8042,#8043,#8044,#8045));
#2414=EDGE_LOOP('',(#8046));
#2415=EDGE_LOOP('',(#8047));
#2416=EDGE_LOOP('',(#8048,#8049,#8050,#8051));
#2417=EDGE_LOOP('',(#8052,#8053,#8054,#8055));
#2418=EDGE_LOOP('',(#8056,#8057,#8058,#8059));
#2419=EDGE_LOOP('',(#8060,#8061,#8062,#8063));
#2420=EDGE_LOOP('',(#8064));
#2421=EDGE_LOOP('',(#8065));
#2422=EDGE_LOOP('',(#8066,#8067,#8068,#8069));
#2423=EDGE_LOOP('',(#8070));
#2424=EDGE_LOOP('',(#8071));
#2425=EDGE_LOOP('',(#8072));
#2426=EDGE_LOOP('',(#8073,#8074,#8075,#8076));
#2427=EDGE_LOOP('',(#8077,#8078,#8079,#8080));
#2428=EDGE_LOOP('',(#8081,#8082,#8083,#8084));
#2429=EDGE_LOOP('',(#8085));
#2430=EDGE_LOOP('',(#8086));
#2431=EDGE_LOOP('',(#8087,#8088,#8089,#8090));
#2432=EDGE_LOOP('',(#8091,#8092,#8093,#8094));
#2433=EDGE_LOOP('',(#8095,#8096,#8097,#8098));
#2434=EDGE_LOOP('',(#8099));
#2435=EDGE_LOOP('',(#8100,#8101,#8102,#8103));
#2436=EDGE_LOOP('',(#8104,#8105,#8106,#8107));
#2437=EDGE_LOOP('',(#8108,#8109,#8110,#8111));
#2438=EDGE_LOOP('',(#8112,#8113,#8114,#8115));
#2439=EDGE_LOOP('',(#8116,#8117,#8118,#8119));
#2440=EDGE_LOOP('',(#8120,#8121,#8122,#8123));
#2441=EDGE_LOOP('',(#8124,#8125,#8126,#8127,#8128,#8129));
#2442=EDGE_LOOP('',(#8130,#8131,#8132,#8133,#8134,#8135));
#2443=EDGE_LOOP('',(#8136,#8137,#8138,#8139));
#2444=EDGE_LOOP('',(#8140,#8141,#8142,#8143));
#2445=EDGE_LOOP('',(#8144,#8145,#8146,#8147));
#2446=EDGE_LOOP('',(#8148,#8149,#8150,#8151));
#2447=EDGE_LOOP('',(#8152,#8153,#8154,#8155));
#2448=EDGE_LOOP('',(#8156,#8157,#8158,#8159));
#2449=EDGE_LOOP('',(#8160,#8161,#8162,#8163,#8164,#8165));
#2450=EDGE_LOOP('',(#8166,#8167,#8168,#8169,#8170,#8171));
#2451=EDGE_LOOP('',(#8172));
#2452=EDGE_LOOP('',(#8173));
#2453=EDGE_LOOP('',(#8174,#8175,#8176,#8177));
#2454=EDGE_LOOP('',(#8178,#8179,#8180,#8181));
#2455=EDGE_LOOP('',(#8182,#8183,#8184,#8185));
#2456=EDGE_LOOP('',(#8186));
#2457=EDGE_LOOP('',(#8187));
#2458=EDGE_LOOP('',(#8188,#8189,#8190,#8191));
#2459=EDGE_LOOP('',(#8192,#8193,#8194,#8195));
#2460=LINE('',#13365,#3106);
#2461=LINE('',#13371,#3107);
#2462=LINE('',#13377,#3108);
#2463=LINE('',#13383,#3109);
#2464=LINE('',#13389,#3110);
#2465=LINE('',#13395,#3111);
#2466=LINE('',#13401,#3112);
#2467=LINE('',#13407,#3113);
#2468=LINE('',#13413,#3114);
#2469=LINE('',#13419,#3115);
#2470=LINE('',#13425,#3116);
#2471=LINE('',#13431,#3117);
#2472=LINE('',#13436,#3118);
#2473=LINE('',#13438,#3119);
#2474=LINE('',#13440,#3120);
#2475=LINE('',#13441,#3121);
#2476=LINE('',#13444,#3122);
#2477=LINE('',#13446,#3123);
#2478=LINE('',#13447,#3124);
#2479=LINE('',#13450,#3125);
#2480=LINE('',#13452,#3126);
#2481=LINE('',#13453,#3127);
#2482=LINE('',#13455,#3128);
#2483=LINE('',#13456,#3129);
#2484=LINE('',#13464,#3130);
#2485=LINE('',#13471,#3131);
#2486=LINE('',#13478,#3132);
#2487=LINE('',#13487,#3133);
#2488=LINE('',#13496,#3134);
#2489=LINE('',#13505,#3135);
#2490=LINE('',#13513,#3136);
#2491=LINE('',#13517,#3137);
#2492=LINE('',#13521,#3138);
#2493=LINE('',#13525,#3139);
#2494=LINE('',#13529,#3140);
#2495=LINE('',#13531,#3141);
#2496=LINE('',#13533,#3142);
#2497=LINE('',#13534,#3143);
#2498=LINE('',#13537,#3144);
#2499=LINE('',#13539,#3145);
#2500=LINE('',#13540,#3146);
#2501=LINE('',#13543,#3147);
#2502=LINE('',#13545,#3148);
#2503=LINE('',#13546,#3149);
#2504=LINE('',#13548,#3150);
#2505=LINE('',#13549,#3151);
#2506=LINE('',#13557,#3152);
#2507=LINE('',#13563,#3153);
#2508=LINE('',#13572,#3154);
#2509=LINE('',#13578,#3155);
#2510=LINE('',#13587,#3156);
#2511=LINE('',#13594,#3157);
#2512=LINE('',#13601,#3158);
#2513=LINE('',#13610,#3159);
#2514=LINE('',#13619,#3160);
#2515=LINE('',#13628,#3161);
#2516=LINE('',#13636,#3162);
#2517=LINE('',#13640,#3163);
#2518=LINE('',#13644,#3164);
#2519=LINE('',#13648,#3165);
#2520=LINE('',#13652,#3166);
#2521=LINE('',#13654,#3167);
#2522=LINE('',#13656,#3168);
#2523=LINE('',#13657,#3169);
#2524=LINE('',#13660,#3170);
#2525=LINE('',#13662,#3171);
#2526=LINE('',#13663,#3172);
#2527=LINE('',#13666,#3173);
#2528=LINE('',#13668,#3174);
#2529=LINE('',#13669,#3175);
#2530=LINE('',#13671,#3176);
#2531=LINE('',#13672,#3177);
#2532=LINE('',#13680,#3178);
#2533=LINE('',#13686,#3179);
#2534=LINE('',#13695,#3180);
#2535=LINE('',#13701,#3181);
#2536=LINE('',#13710,#3182);
#2537=LINE('',#13717,#3183);
#2538=LINE('',#13724,#3184);
#2539=LINE('',#13731,#3185);
#2540=LINE('',#13738,#3186);
#2541=LINE('',#13747,#3187);
#2542=LINE('',#13756,#3188);
#2543=LINE('',#13765,#3189);
#2544=LINE('',#13773,#3190);
#2545=LINE('',#13777,#3191);
#2546=LINE('',#13781,#3192);
#2547=LINE('',#13785,#3193);
#2548=LINE('',#13789,#3194);
#2549=LINE('',#13791,#3195);
#2550=LINE('',#13793,#3196);
#2551=LINE('',#13794,#3197);
#2552=LINE('',#13797,#3198);
#2553=LINE('',#13799,#3199);
#2554=LINE('',#13800,#3200);
#2555=LINE('',#13803,#3201);
#2556=LINE('',#13805,#3202);
#2557=LINE('',#13806,#3203);
#2558=LINE('',#13808,#3204);
#2559=LINE('',#13809,#3205);
#2560=LINE('',#13816,#3206);
#2561=LINE('',#13818,#3207);
#2562=LINE('',#13820,#3208);
#2563=LINE('',#13821,#3209);
#2564=LINE('',#13824,#3210);
#2565=LINE('',#13826,#3211);
#2566=LINE('',#13827,#3212);
#2567=LINE('',#13830,#3213);
#2568=LINE('',#13832,#3214);
#2569=LINE('',#13833,#3215);
#2570=LINE('',#13835,#3216);
#2571=LINE('',#13836,#3217);
#2572=LINE('',#13843,#3218);
#2573=LINE('',#13845,#3219);
#2574=LINE('',#13847,#3220);
#2575=LINE('',#13848,#3221);
#2576=LINE('',#13851,#3222);
#2577=LINE('',#13853,#3223);
#2578=LINE('',#13854,#3224);
#2579=LINE('',#13857,#3225);
#2580=LINE('',#13859,#3226);
#2581=LINE('',#13860,#3227);
#2582=LINE('',#13862,#3228);
#2583=LINE('',#13863,#3229);
#2584=LINE('',#13872,#3230);
#2585=LINE('',#13878,#3231);
#2586=LINE('',#13887,#3232);
#2587=LINE('',#13889,#3233);
#2588=LINE('',#13894,#3234);
#2589=LINE('',#13897,#3235);
#2590=LINE('',#13901,#3236);
#2591=LINE('',#13904,#3237);
#2592=LINE('',#13906,#3238);
#2593=LINE('',#13907,#3239);
#2594=LINE('',#13911,#3240);
#2595=LINE('',#13913,#3241);
#2596=LINE('',#13916,#3242);
#2597=LINE('',#13917,#3243);
#2598=LINE('',#13921,#3244);
#2599=LINE('',#13923,#3245);
#2600=LINE('',#13925,#3246);
#2601=LINE('',#13926,#3247);
#2602=LINE('',#13932,#3248);
#2603=LINE('',#13934,#3249);
#2604=LINE('',#13935,#3250);
#2605=LINE('',#13937,#3251);
#2606=LINE('',#13939,#3252);
#2607=LINE('',#13940,#3253);
#2608=LINE('',#13949,#3254);
#2609=LINE('',#13951,#3255);
#2610=LINE('',#13953,#3256);
#2611=LINE('',#13954,#3257);
#2612=LINE('',#13957,#3258);
#2613=LINE('',#13959,#3259);
#2614=LINE('',#13960,#3260);
#2615=LINE('',#13963,#3261);
#2616=LINE('',#13965,#3262);
#2617=LINE('',#13966,#3263);
#2618=LINE('',#13968,#3264);
#2619=LINE('',#13969,#3265);
#2620=LINE('',#13974,#3266);
#2621=LINE('',#13978,#3267);
#2622=LINE('',#13982,#3268);
#2623=LINE('',#13983,#3269);
#2624=LINE('',#13984,#3270);
#2625=LINE('',#13987,#3271);
#2626=LINE('',#13988,#3272);
#2627=LINE('',#13991,#3273);
#2628=LINE('',#13992,#3274);
#2629=LINE('',#13994,#3275);
#2630=LINE('',#14001,#3276);
#2631=LINE('',#14056,#3277);
#2632=LINE('',#14128,#3278);
#2633=LINE('',#14173,#3279);
#2634=LINE('',#14341,#3280);
#2635=LINE('',#14412,#3281);
#2636=LINE('',#14415,#3282);
#2637=LINE('',#14486,#3283);
#2638=LINE('',#14496,#3284);
#2639=LINE('',#14501,#3285);
#2640=LINE('',#14509,#3286);
#2641=LINE('',#14515,#3287);
#2642=LINE('',#14523,#3288);
#2643=LINE('',#14525,#3289);
#2644=LINE('',#14527,#3290);
#2645=LINE('',#14528,#3291);
#2646=LINE('',#14531,#3292);
#2647=LINE('',#14533,#3293);
#2648=LINE('',#14534,#3294);
#2649=LINE('',#14537,#3295);
#2650=LINE('',#14539,#3296);
#2651=LINE('',#14540,#3297);
#2652=LINE('',#14543,#3298);
#2653=LINE('',#14545,#3299);
#2654=LINE('',#14546,#3300);
#2655=LINE('',#14549,#3301);
#2656=LINE('',#14551,#3302);
#2657=LINE('',#14552,#3303);
#2658=LINE('',#14554,#3304);
#2659=LINE('',#14555,#3305);
#2660=LINE('',#14567,#3306);
#2661=LINE('',#14571,#3307);
#2662=LINE('',#14575,#3308);
#2663=LINE('',#14582,#3309);
#2664=LINE('',#14584,#3310);
#2665=LINE('',#14590,#3311);
#2666=LINE('',#14599,#3312);
#2667=LINE('',#14608,#3313);
#2668=LINE('',#14617,#3314);
#2669=LINE('',#14625,#3315);
#2670=LINE('',#14629,#3316);
#2671=LINE('',#14633,#3317);
#2672=LINE('',#14637,#3318);
#2673=LINE('',#14641,#3319);
#2674=LINE('',#14643,#3320);
#2675=LINE('',#14645,#3321);
#2676=LINE('',#14646,#3322);
#2677=LINE('',#14649,#3323);
#2678=LINE('',#14651,#3324);
#2679=LINE('',#14652,#3325);
#2680=LINE('',#14655,#3326);
#2681=LINE('',#14657,#3327);
#2682=LINE('',#14658,#3328);
#2683=LINE('',#14661,#3329);
#2684=LINE('',#14663,#3330);
#2685=LINE('',#14664,#3331);
#2686=LINE('',#14667,#3332);
#2687=LINE('',#14669,#3333);
#2688=LINE('',#14670,#3334);
#2689=LINE('',#14673,#3335);
#2690=LINE('',#14675,#3336);
#2691=LINE('',#14676,#3337);
#2692=LINE('',#14679,#3338);
#2693=LINE('',#14681,#3339);
#2694=LINE('',#14682,#3340);
#2695=LINE('',#14685,#3341);
#2696=LINE('',#14687,#3342);
#2697=LINE('',#14688,#3343);
#2698=LINE('',#14691,#3344);
#2699=LINE('',#14693,#3345);
#2700=LINE('',#14694,#3346);
#2701=LINE('',#14697,#3347);
#2702=LINE('',#14699,#3348);
#2703=LINE('',#14700,#3349);
#2704=LINE('',#14703,#3350);
#2705=LINE('',#14705,#3351);
#2706=LINE('',#14706,#3352);
#2707=LINE('',#14708,#3353);
#2708=LINE('',#14709,#3354);
#2709=LINE('',#14719,#3355);
#2710=LINE('',#14723,#3356);
#2711=LINE('',#14727,#3357);
#2712=LINE('',#14734,#3358);
#2713=LINE('',#14738,#3359);
#2714=LINE('',#14742,#3360);
#2715=LINE('',#14747,#3361);
#2716=LINE('',#14749,#3362);
#2717=LINE('',#14751,#3363);
#2718=LINE('',#14752,#3364);
#2719=LINE('',#14755,#3365);
#2720=LINE('',#14757,#3366);
#2721=LINE('',#14758,#3367);
#2722=LINE('',#14761,#3368);
#2723=LINE('',#14763,#3369);
#2724=LINE('',#14764,#3370);
#2725=LINE('',#14767,#3371);
#2726=LINE('',#14769,#3372);
#2727=LINE('',#14770,#3373);
#2728=LINE('',#14773,#3374);
#2729=LINE('',#14775,#3375);
#2730=LINE('',#14776,#3376);
#2731=LINE('',#14778,#3377);
#2732=LINE('',#14779,#3378);
#2733=LINE('',#14787,#3379);
#2734=LINE('',#14789,#3380);
#2735=LINE('',#14791,#3381);
#2736=LINE('',#14792,#3382);
#2737=LINE('',#14797,#3383);
#2738=LINE('',#14798,#3384);
#2739=LINE('',#14801,#3385);
#2740=LINE('',#14803,#3386);
#2741=LINE('',#14804,#3387);
#2742=LINE('',#14806,#3388);
#2743=LINE('',#14811,#3389);
#2744=LINE('',#14820,#3390);
#2745=LINE('',#14841,#3391);
#2746=LINE('',#14896,#3392);
#2747=LINE('',#14901,#3393);
#2748=LINE('',#14907,#3394);
#2749=LINE('',#14915,#3395);
#2750=LINE('',#14936,#3396);
#2751=LINE('',#14991,#3397);
#2752=LINE('',#14996,#3398);
#2753=LINE('',#15002,#3399);
#2754=LINE('',#15011,#3400);
#2755=LINE('',#15017,#3401);
#2756=LINE('',#15029,#3402);
#2757=LINE('',#15033,#3403);
#2758=LINE('',#15037,#3404);
#2759=LINE('',#15042,#3405);
#2760=LINE('',#15053,#3406);
#2761=LINE('',#15066,#3407);
#2762=LINE('',#15077,#3408);
#2763=LINE('',#15081,#3409);
#2764=LINE('',#15083,#3410);
#2765=LINE('',#15084,#3411);
#2766=LINE('',#15090,#3412);
#2767=LINE('',#15092,#3413);
#2768=LINE('',#15093,#3414);
#2769=LINE('',#15095,#3415);
#2770=LINE('',#15101,#3416);
#2771=LINE('',#15138,#3417);
#2772=LINE('',#15141,#3418);
#2773=LINE('',#15148,#3419);
#2774=LINE('',#15151,#3420);
#2775=LINE('',#15160,#3421);
#2776=LINE('',#15171,#3422);
#2777=LINE('',#15175,#3423);
#2778=LINE('',#15183,#3424);
#2779=LINE('',#15189,#3425);
#2780=LINE('',#15198,#3426);
#2781=LINE('',#15204,#3427);
#2782=LINE('',#15213,#3428);
#2783=LINE('',#15219,#3429);
#2784=LINE('',#15227,#3430);
#2785=LINE('',#15229,#3431);
#2786=LINE('',#15231,#3432);
#2787=LINE('',#15233,#3433);
#2788=LINE('',#15235,#3434);
#2789=LINE('',#15237,#3435);
#2790=LINE('',#15239,#3436);
#2791=LINE('',#15240,#3437);
#2792=LINE('',#15243,#3438);
#2793=LINE('',#15245,#3439);
#2794=LINE('',#15246,#3440);
#2795=LINE('',#15249,#3441);
#2796=LINE('',#15250,#3442);
#2797=LINE('',#15253,#3443);
#2798=LINE('',#15254,#3444);
#2799=LINE('',#15257,#3445);
#2800=LINE('',#15258,#3446);
#2801=LINE('',#15262,#3447);
#2802=LINE('',#15263,#3448);
#2803=LINE('',#15265,#3449);
#2804=LINE('',#15266,#3450);
#2805=LINE('',#15268,#3451);
#2806=LINE('',#15270,#3452);
#2807=LINE('',#15272,#3453);
#2808=LINE('',#15278,#3454);
#2809=LINE('',#15280,#3455);
#2810=LINE('',#15282,#3456);
#2811=LINE('',#15283,#3457);
#2812=LINE('',#15286,#3458);
#2813=LINE('',#15288,#3459);
#2814=LINE('',#15289,#3460);
#2815=LINE('',#15292,#3461);
#2816=LINE('',#15294,#3462);
#2817=LINE('',#15295,#3463);
#2818=LINE('',#15298,#3464);
#2819=LINE('',#15300,#3465);
#2820=LINE('',#15301,#3466);
#2821=LINE('',#15304,#3467);
#2822=LINE('',#15306,#3468);
#2823=LINE('',#15307,#3469);
#2824=LINE('',#15309,#3470);
#2825=LINE('',#15310,#3471);
#2826=LINE('',#15318,#3472);
#2827=LINE('',#15322,#3473);
#2828=LINE('',#15326,#3474);
#2829=LINE('',#15334,#3475);
#2830=LINE('',#15340,#3476);
#2831=LINE('',#15345,#3477);
#2832=LINE('',#15349,#3478);
#2833=LINE('',#15353,#3479);
#2834=LINE('',#15356,#3480);
#2835=LINE('',#15359,#3481);
#2836=LINE('',#15360,#3482);
#2837=LINE('',#15363,#3483);
#2838=LINE('',#15366,#3484);
#2839=LINE('',#15373,#3485);
#2840=LINE('',#15379,#3486);
#2841=LINE('',#15388,#3487);
#2842=LINE('',#15394,#3488);
#2843=LINE('',#15403,#3489);
#2844=LINE('',#15409,#3490);
#2845=LINE('',#15418,#3491);
#2846=LINE('',#15424,#3492);
#2847=LINE('',#15442,#3493);
#2848=LINE('',#15448,#3494);
#2849=LINE('',#15452,#3495);
#2850=LINE('',#15458,#3496);
#2851=LINE('',#15463,#3497);
#2852=LINE('',#15478,#3498);
#2853=LINE('',#15487,#3499);
#2854=LINE('',#15491,#3500);
#2855=LINE('',#15495,#3501);
#2856=LINE('',#15498,#3502);
#2857=LINE('',#15651,#3503);
#2858=LINE('',#15947,#3504);
#2859=LINE('',#15989,#3505);
#2860=LINE('',#15994,#3506);
#2861=LINE('',#16003,#3507);
#2862=LINE('',#16008,#3508);
#2863=LINE('',#16027,#3509);
#2864=LINE('',#16034,#3510);
#2865=LINE('',#16040,#3511);
#2866=LINE('',#16042,#3512);
#2867=LINE('',#16044,#3513);
#2868=LINE('',#16045,#3514);
#2869=LINE('',#16049,#3515);
#2870=LINE('',#16051,#3516);
#2871=LINE('',#16053,#3517);
#2872=LINE('',#16054,#3518);
#2873=LINE('',#16056,#3519);
#2874=LINE('',#16057,#3520);
#2875=LINE('',#16059,#3521);
#2876=LINE('',#16064,#3522);
#2877=LINE('',#16069,#3523);
#2878=LINE('',#16071,#3524);
#2879=LINE('',#16073,#3525);
#2880=LINE('',#16074,#3526);
#2881=LINE('',#16077,#3527);
#2882=LINE('',#16079,#3528);
#2883=LINE('',#16080,#3529);
#2884=LINE('',#16083,#3530);
#2885=LINE('',#16085,#3531);
#2886=LINE('',#16086,#3532);
#2887=LINE('',#16088,#3533);
#2888=LINE('',#16090,#3534);
#2889=LINE('',#16095,#3535);
#2890=LINE('',#16101,#3536);
#2891=LINE('',#16107,#3537);
#2892=LINE('',#16113,#3538);
#2893=LINE('',#16118,#3539);
#2894=LINE('',#16120,#3540);
#2895=LINE('',#16122,#3541);
#2896=LINE('',#16123,#3542);
#2897=LINE('',#16126,#3543);
#2898=LINE('',#16128,#3544);
#2899=LINE('',#16129,#3545);
#2900=LINE('',#16132,#3546);
#2901=LINE('',#16133,#3547);
#2902=LINE('',#16135,#3548);
#2903=LINE('',#16136,#3549);
#2904=LINE('',#16138,#3550);
#2905=LINE('',#16139,#3551);
#2906=LINE('',#16147,#3552);
#2907=LINE('',#16153,#3553);
#2908=LINE('',#16158,#3554);
#2909=LINE('',#16160,#3555);
#2910=LINE('',#16162,#3556);
#2911=LINE('',#16163,#3557);
#2912=LINE('',#16166,#3558);
#2913=LINE('',#16168,#3559);
#2914=LINE('',#16169,#3560);
#2915=LINE('',#16172,#3561);
#2916=LINE('',#16174,#3562);
#2917=LINE('',#16175,#3563);
#2918=LINE('',#16177,#3564);
#2919=LINE('',#16178,#3565);
#2920=LINE('',#16186,#3566);
#2921=LINE('',#16196,#3567);
#2922=LINE('',#16202,#3568);
#2923=LINE('',#16209,#3569);
#2924=LINE('',#16215,#3570);
#2925=LINE('',#16224,#3571);
#2926=LINE('',#16230,#3572);
#2927=LINE('',#16239,#3573);
#2928=LINE('',#16245,#3574);
#2929=LINE('',#16254,#3575);
#2930=LINE('',#16258,#3576);
#2931=LINE('',#16262,#3577);
#2932=LINE('',#16266,#3578);
#2933=LINE('',#16270,#3579);
#2934=LINE('',#16274,#3580);
#2935=LINE('',#16278,#3581);
#2936=LINE('',#16282,#3582);
#2937=LINE('',#16286,#3583);
#2938=LINE('',#16290,#3584);
#2939=LINE('',#16294,#3585);
#2940=LINE('',#16298,#3586);
#2941=LINE('',#16302,#3587);
#2942=LINE('',#16306,#3588);
#2943=LINE('',#16310,#3589);
#2944=LINE('',#16314,#3590);
#2945=LINE('',#16316,#3591);
#2946=LINE('',#16318,#3592);
#2947=LINE('',#16320,#3593);
#2948=LINE('',#16322,#3594);
#2949=LINE('',#16324,#3595);
#2950=LINE('',#16325,#3596);
#2951=LINE('',#16327,#3597);
#2952=LINE('',#16329,#3598);
#2953=LINE('',#16331,#3599);
#2954=LINE('',#16333,#3600);
#2955=LINE('',#16335,#3601);
#2956=LINE('',#16336,#3602);
#2957=LINE('',#16339,#3603);
#2958=LINE('',#16341,#3604);
#2959=LINE('',#16343,#3605);
#2960=LINE('',#16345,#3606);
#2961=LINE('',#16346,#3607);
#2962=LINE('',#16348,#3608);
#2963=LINE('',#16350,#3609);
#2964=LINE('',#16352,#3610);
#2965=LINE('',#16354,#3611);
#2966=LINE('',#16355,#3612);
#2967=LINE('',#16358,#3613);
#2968=LINE('',#16359,#3614);
#2969=LINE('',#16362,#3615);
#2970=LINE('',#16363,#3616);
#2971=LINE('',#16366,#3617);
#2972=LINE('',#16367,#3618);
#2973=LINE('',#16370,#3619);
#2974=LINE('',#16371,#3620);
#2975=LINE('',#16373,#3621);
#2976=LINE('',#16376,#3622);
#2977=LINE('',#16377,#3623);
#2978=LINE('',#16380,#3624);
#2979=LINE('',#16381,#3625);
#2980=LINE('',#16384,#3626);
#2981=LINE('',#16385,#3627);
#2982=LINE('',#16388,#3628);
#2983=LINE('',#16389,#3629);
#2984=LINE('',#16391,#3630);
#2985=LINE('',#16397,#3631);
#2986=LINE('',#16399,#3632);
#2987=LINE('',#16401,#3633);
#2988=LINE('',#16402,#3634);
#2989=LINE('',#16405,#3635);
#2990=LINE('',#16407,#3636);
#2991=LINE('',#16408,#3637);
#2992=LINE('',#16411,#3638);
#2993=LINE('',#16413,#3639);
#2994=LINE('',#16414,#3640);
#2995=LINE('',#16417,#3641);
#2996=LINE('',#16419,#3642);
#2997=LINE('',#16420,#3643);
#2998=LINE('',#16423,#3644);
#2999=LINE('',#16425,#3645);
#3000=LINE('',#16426,#3646);
#3001=LINE('',#16429,#3647);
#3002=LINE('',#16431,#3648);
#3003=LINE('',#16432,#3649);
#3004=LINE('',#16435,#3650);
#3005=LINE('',#16437,#3651);
#3006=LINE('',#16438,#3652);
#3007=LINE('',#16440,#3653);
#3008=LINE('',#16441,#3654);
#3009=LINE('',#16448,#3655);
#3010=LINE('',#16450,#3656);
#3011=LINE('',#16452,#3657);
#3012=LINE('',#16453,#3658);
#3013=LINE('',#16456,#3659);
#3014=LINE('',#16458,#3660);
#3015=LINE('',#16459,#3661);
#3016=LINE('',#16462,#3662);
#3017=LINE('',#16464,#3663);
#3018=LINE('',#16465,#3664);
#3019=LINE('',#16468,#3665);
#3020=LINE('',#16470,#3666);
#3021=LINE('',#16471,#3667);
#3022=LINE('',#16474,#3668);
#3023=LINE('',#16476,#3669);
#3024=LINE('',#16477,#3670);
#3025=LINE('',#16480,#3671);
#3026=LINE('',#16482,#3672);
#3027=LINE('',#16483,#3673);
#3028=LINE('',#16486,#3674);
#3029=LINE('',#16488,#3675);
#3030=LINE('',#16489,#3676);
#3031=LINE('',#16491,#3677);
#3032=LINE('',#16492,#3678);
#3033=LINE('',#16502,#3679);
#3034=LINE('',#16504,#3680);
#3035=LINE('',#16506,#3681);
#3036=LINE('',#16507,#3682);
#3037=LINE('',#16510,#3683);
#3038=LINE('',#16512,#3684);
#3039=LINE('',#16513,#3685);
#3040=LINE('',#16516,#3686);
#3041=LINE('',#16518,#3687);
#3042=LINE('',#16519,#3688);
#3043=LINE('',#16522,#3689);
#3044=LINE('',#16524,#3690);
#3045=LINE('',#16525,#3691);
#3046=LINE('',#16528,#3692);
#3047=LINE('',#16530,#3693);
#3048=LINE('',#16531,#3694);
#3049=LINE('',#16533,#3695);
#3050=LINE('',#16534,#3696);
#3051=LINE('',#16546,#3697);
#3052=LINE('',#16550,#3698);
#3053=LINE('',#16554,#3699);
#3054=LINE('',#16561,#3700);
#3055=LINE('',#16563,#3701);
#3056=LINE('',#16569,#3702);
#3057=LINE('',#16573,#3703);
#3058=LINE('',#16580,#3704);
#3059=LINE('',#16590,#3705);
#3060=LINE('',#16594,#3706);
#3061=LINE('',#16598,#3707);
#3062=LINE('',#16605,#3708);
#3063=LINE('',#16609,#3709);
#3064=LINE('',#16613,#3710);
#3065=LINE('',#16618,#3711);
#3066=LINE('',#16620,#3712);
#3067=LINE('',#16622,#3713);
#3068=LINE('',#16623,#3714);
#3069=LINE('',#16626,#3715);
#3070=LINE('',#16628,#3716);
#3071=LINE('',#16629,#3717);
#3072=LINE('',#16632,#3718);
#3073=LINE('',#16634,#3719);
#3074=LINE('',#16635,#3720);
#3075=LINE('',#16638,#3721);
#3076=LINE('',#16640,#3722);
#3077=LINE('',#16641,#3723);
#3078=LINE('',#16644,#3724);
#3079=LINE('',#16646,#3725);
#3080=LINE('',#16647,#3726);
#3081=LINE('',#16649,#3727);
#3082=LINE('',#16650,#3728);
#3083=LINE('',#16694,#3729);
#3084=LINE('',#16696,#3730);
#3085=LINE('',#16698,#3731);
#3086=LINE('',#16699,#3732);
#3087=LINE('',#16702,#3733);
#3088=LINE('',#16704,#3734);
#3089=LINE('',#16705,#3735);
#3090=LINE('',#16708,#3736);
#3091=LINE('',#16710,#3737);
#3092=LINE('',#16711,#3738);
#3093=LINE('',#16714,#3739);
#3094=LINE('',#16716,#3740);
#3095=LINE('',#16717,#3741);
#3096=LINE('',#16720,#3742);
#3097=LINE('',#16722,#3743);
#3098=LINE('',#16723,#3744);
#3099=LINE('',#16725,#3745);
#3100=LINE('',#16726,#3746);
#3101=LINE('',#16738,#3747);
#3102=LINE('',#16742,#3748);
#3103=LINE('',#16746,#3749);
#3104=LINE('',#16753,#3750);
#3105=LINE('',#16755,#3751);
#3106=VECTOR('',#10576,0.210000000000001);
#3107=VECTOR('',#10583,0.21);
#3108=VECTOR('',#10590,0.21);
#3109=VECTOR('',#10597,0.210000000000001);
#3110=VECTOR('',#10604,0.21);
#3111=VECTOR('',#10611,0.21);
#3112=VECTOR('',#10618,0.21);
#3113=VECTOR('',#10625,0.21);
#3114=VECTOR('',#10632,0.21);
#3115=VECTOR('',#10639,0.21);
#3116=VECTOR('',#10646,0.21);
#3117=VECTOR('',#10653,0.21);
#3118=VECTOR('',#10658,1.);
#3119=VECTOR('',#10659,1.);
#3120=VECTOR('',#10660,1.);
#3121=VECTOR('',#10661,1.);
#3122=VECTOR('',#10664,1.);
#3123=VECTOR('',#10665,1.);
#3124=VECTOR('',#10666,1.);
#3125=VECTOR('',#10669,1.);
#3126=VECTOR('',#10670,1.);
#3127=VECTOR('',#10671,1.);
#3128=VECTOR('',#10674,1.);
#3129=VECTOR('',#10675,1.);
#3130=VECTOR('',#10686,0.34);
#3131=VECTOR('',#10695,0.34);
#3132=VECTOR('',#10704,0.5);
#3133=VECTOR('',#10715,0.5);
#3134=VECTOR('',#10726,0.5);
#3135=VECTOR('',#10737,0.5);
#3136=VECTOR('',#10748,0.275);
#3137=VECTOR('',#10753,0.275);
#3138=VECTOR('',#10758,0.275);
#3139=VECTOR('',#10763,0.275);
#3140=VECTOR('',#10766,1.);
#3141=VECTOR('',#10767,1.);
#3142=VECTOR('',#10768,1.);
#3143=VECTOR('',#10769,1.);
#3144=VECTOR('',#10772,1.);
#3145=VECTOR('',#10773,1.);
#3146=VECTOR('',#10774,1.);
#3147=VECTOR('',#10777,1.);
#3148=VECTOR('',#10778,1.);
#3149=VECTOR('',#10779,1.);
#3150=VECTOR('',#10782,1.);
#3151=VECTOR('',#10783,1.);
#3152=VECTOR('',#10794,0.425);
#3153=VECTOR('',#10801,0.645);
#3154=VECTOR('',#10814,0.425);
#3155=VECTOR('',#10821,0.645);
#3156=VECTOR('',#10834,0.34);
#3157=VECTOR('',#10843,0.34);
#3158=VECTOR('',#10852,0.5);
#3159=VECTOR('',#10863,0.5);
#3160=VECTOR('',#10874,0.5);
#3161=VECTOR('',#10885,0.5);
#3162=VECTOR('',#10896,0.275);
#3163=VECTOR('',#10901,0.275);
#3164=VECTOR('',#10906,0.275);
#3165=VECTOR('',#10911,0.275);
#3166=VECTOR('',#10914,1.);
#3167=VECTOR('',#10915,1.);
#3168=VECTOR('',#10916,1.);
#3169=VECTOR('',#10917,1.);
#3170=VECTOR('',#10920,1.);
#3171=VECTOR('',#10921,1.);
#3172=VECTOR('',#10922,1.);
#3173=VECTOR('',#10925,1.);
#3174=VECTOR('',#10926,1.);
#3175=VECTOR('',#10927,1.);
#3176=VECTOR('',#10930,1.);
#3177=VECTOR('',#10931,1.);
#3178=VECTOR('',#10942,0.425);
#3179=VECTOR('',#10949,0.645);
#3180=VECTOR('',#10962,0.425);
#3181=VECTOR('',#10969,0.645);
#3182=VECTOR('',#10982,0.164999999999999);
#3183=VECTOR('',#10991,0.164999999999999);
#3184=VECTOR('',#11000,0.165);
#3185=VECTOR('',#11009,0.164999999999999);
#3186=VECTOR('',#11018,0.5);
#3187=VECTOR('',#11029,0.5);
#3188=VECTOR('',#11040,0.5);
#3189=VECTOR('',#11051,0.5);
#3190=VECTOR('',#11062,0.274999999999999);
#3191=VECTOR('',#11067,0.275);
#3192=VECTOR('',#11072,0.275);
#3193=VECTOR('',#11077,0.274999999999999);
#3194=VECTOR('',#11080,1.);
#3195=VECTOR('',#11081,1.);
#3196=VECTOR('',#11082,1.);
#3197=VECTOR('',#11083,1.);
#3198=VECTOR('',#11086,1.);
#3199=VECTOR('',#11087,1.);
#3200=VECTOR('',#11088,1.);
#3201=VECTOR('',#11091,1.);
#3202=VECTOR('',#11092,1.);
#3203=VECTOR('',#11093,1.);
#3204=VECTOR('',#11096,1.);
#3205=VECTOR('',#11097,1.);
#3206=VECTOR('',#11106,1.);
#3207=VECTOR('',#11107,1.);
#3208=VECTOR('',#11108,1.);
#3209=VECTOR('',#11109,1.);
#3210=VECTOR('',#11112,1.);
#3211=VECTOR('',#11113,1.);
#3212=VECTOR('',#11114,1.);
#3213=VECTOR('',#11117,1.);
#3214=VECTOR('',#11118,1.);
#3215=VECTOR('',#11119,1.);
#3216=VECTOR('',#11122,1.);
#3217=VECTOR('',#11123,1.);
#3218=VECTOR('',#11132,1.);
#3219=VECTOR('',#11133,1.);
#3220=VECTOR('',#11134,1.);
#3221=VECTOR('',#11135,1.);
#3222=VECTOR('',#11138,1.);
#3223=VECTOR('',#11139,1.);
#3224=VECTOR('',#11140,1.);
#3225=VECTOR('',#11143,1.);
#3226=VECTOR('',#11144,1.);
#3227=VECTOR('',#11145,1.);
#3228=VECTOR('',#11148,1.);
#3229=VECTOR('',#11149,1.);
#3230=VECTOR('',#11162,2.05);
#3231=VECTOR('',#11169,2.05);
#3232=VECTOR('',#11178,1.);
#3233=VECTOR('',#11179,1.);
#3234=VECTOR('',#11184,1.);
#3235=VECTOR('',#11187,1.);
#3236=VECTOR('',#11190,1.);
#3237=VECTOR('',#11193,1.);
#3238=VECTOR('',#11196,1.);
#3239=VECTOR('',#11197,1.);
#3240=VECTOR('',#11200,1.);
#3241=VECTOR('',#11201,1.);
#3242=VECTOR('',#11206,1.);
#3243=VECTOR('',#11207,1.);
#3244=VECTOR('',#11210,1.);
#3245=VECTOR('',#11211,1.);
#3246=VECTOR('',#11212,1.);
#3247=VECTOR('',#11213,1.);
#3248=VECTOR('',#11218,1.);
#3249=VECTOR('',#11219,1.);
#3250=VECTOR('',#11220,1.);
#3251=VECTOR('',#11221,1.);
#3252=VECTOR('',#11222,1.);
#3253=VECTOR('',#11223,1.);
#3254=VECTOR('',#11236,1.);
#3255=VECTOR('',#11237,1.);
#3256=VECTOR('',#11238,1.);
#3257=VECTOR('',#11239,1.);
#3258=VECTOR('',#11242,1.);
#3259=VECTOR('',#11243,1.);
#3260=VECTOR('',#11244,1.);
#3261=VECTOR('',#11247,1.);
#3262=VECTOR('',#11248,1.);
#3263=VECTOR('',#11249,1.);
#3264=VECTOR('',#11252,1.);
#3265=VECTOR('',#11253,1.);
#3266=VECTOR('',#11260,0.65);
#3267=VECTOR('',#11265,0.65);
#3268=VECTOR('',#11268,1.);
#3269=VECTOR('',#11269,1.);
#3270=VECTOR('',#11270,1.);
#3271=VECTOR('',#11273,1.);
#3272=VECTOR('',#11274,1.);
#3273=VECTOR('',#11277,1.);
#3274=VECTOR('',#11278,1.);
#3275=VECTOR('',#11281,1.);
#3276=VECTOR('',#11290,1.8);
#3277=VECTOR('',#11307,0.25);
#3278=VECTOR('',#11310,0.25);
#3279=VECTOR('',#11315,1.65);
#3280=VECTOR('',#11320,0.25);
#3281=VECTOR('',#11323,0.25);
#3282=VECTOR('',#11326,0.25);
#3283=VECTOR('',#11329,0.25);
#3284=VECTOR('',#11342,1.75);
#3285=VECTOR('',#11349,1.);
#3286=VECTOR('',#11360,0.42);
#3287=VECTOR('',#11367,0.8);
#3288=VECTOR('',#11378,1.);
#3289=VECTOR('',#11379,1.);
#3290=VECTOR('',#11380,1.);
#3291=VECTOR('',#11381,1.);
#3292=VECTOR('',#11384,1.);
#3293=VECTOR('',#11385,1.);
#3294=VECTOR('',#11386,1.);
#3295=VECTOR('',#11389,1.);
#3296=VECTOR('',#11390,1.);
#3297=VECTOR('',#11391,1.);
#3298=VECTOR('',#11394,1.);
#3299=VECTOR('',#11395,1.);
#3300=VECTOR('',#11396,1.);
#3301=VECTOR('',#11399,1.);
#3302=VECTOR('',#11400,1.);
#3303=VECTOR('',#11401,1.);
#3304=VECTOR('',#11404,1.);
#3305=VECTOR('',#11405,1.);
#3306=VECTOR('',#11422,0.625);
#3307=VECTOR('',#11427,0.65);
#3308=VECTOR('',#11432,0.635);
#3309=VECTOR('',#11441,0.41);
#3310=VECTOR('',#11444,0.4);
#3311=VECTOR('',#11451,0.375);
#3312=VECTOR('',#11462,0.375);
#3313=VECTOR('',#11473,0.375);
#3314=VECTOR('',#11484,0.375);
#3315=VECTOR('',#11495,0.225);
#3316=VECTOR('',#11500,0.225);
#3317=VECTOR('',#11505,0.225);
#3318=VECTOR('',#11510,0.225000000000001);
#3319=VECTOR('',#11513,1.);
#3320=VECTOR('',#11514,1.);
#3321=VECTOR('',#11515,1.);
#3322=VECTOR('',#11516,1.);
#3323=VECTOR('',#11519,1.);
#3324=VECTOR('',#11520,1.);
#3325=VECTOR('',#11521,1.);
#3326=VECTOR('',#11524,1.);
#3327=VECTOR('',#11525,1.);
#3328=VECTOR('',#11526,1.);
#3329=VECTOR('',#11529,1.);
#3330=VECTOR('',#11530,1.);
#3331=VECTOR('',#11531,1.);
#3332=VECTOR('',#11534,1.);
#3333=VECTOR('',#11535,1.);
#3334=VECTOR('',#11536,1.);
#3335=VECTOR('',#11539,1.);
#3336=VECTOR('',#11540,1.);
#3337=VECTOR('',#11541,1.);
#3338=VECTOR('',#11544,1.);
#3339=VECTOR('',#11545,1.);
#3340=VECTOR('',#11546,1.);
#3341=VECTOR('',#11549,1.);
#3342=VECTOR('',#11550,1.);
#3343=VECTOR('',#11551,1.);
#3344=VECTOR('',#11554,1.);
#3345=VECTOR('',#11555,1.);
#3346=VECTOR('',#11556,1.);
#3347=VECTOR('',#11559,1.);
#3348=VECTOR('',#11560,1.);
#3349=VECTOR('',#11561,1.);
#3350=VECTOR('',#11564,1.);
#3351=VECTOR('',#11565,1.);
#3352=VECTOR('',#11566,1.);
#3353=VECTOR('',#11569,1.);
#3354=VECTOR('',#11570,1.);
#3355=VECTOR('',#11585,0.325);
#3356=VECTOR('',#11590,0.35);
#3357=VECTOR('',#11595,0.335);
#3358=VECTOR('',#11604,0.21);
#3359=VECTOR('',#11609,0.2);
#3360=VECTOR('',#11614,0.18);
#3361=VECTOR('',#11619,1.);
#3362=VECTOR('',#11620,1.);
#3363=VECTOR('',#11621,1.);
#3364=VECTOR('',#11622,1.);
#3365=VECTOR('',#11625,1.);
#3366=VECTOR('',#11626,1.);
#3367=VECTOR('',#11627,1.);
#3368=VECTOR('',#11630,1.);
#3369=VECTOR('',#11631,1.);
#3370=VECTOR('',#11632,1.);
#3371=VECTOR('',#11635,1.);
#3372=VECTOR('',#11636,1.);
#3373=VECTOR('',#11637,1.);
#3374=VECTOR('',#11640,1.);
#3375=VECTOR('',#11641,1.);
#3376=VECTOR('',#11642,1.);
#3377=VECTOR('',#11645,1.);
#3378=VECTOR('',#11646,1.);
#3379=VECTOR('',#11657,1.);
#3380=VECTOR('',#11658,1.);
#3381=VECTOR('',#11659,1.);
#3382=VECTOR('',#11660,1.);
#3383=VECTOR('',#11665,1.);
#3384=VECTOR('',#11666,1.);
#3385=VECTOR('',#11669,1.);
#3386=VECTOR('',#11670,1.);
#3387=VECTOR('',#11671,1.);
#3388=VECTOR('',#11674,1.);
#3389=VECTOR('',#11679,1.);
#3390=VECTOR('',#11692,1.);
#3391=VECTOR('',#11699,0.21);
#3392=VECTOR('',#11704,1.);
#3393=VECTOR('',#11709,1.005);
#3394=VECTOR('',#11716,1.5);
#3395=VECTOR('',#11727,1.);
#3396=VECTOR('',#11734,0.21);
#3397=VECTOR('',#11739,1.);
#3398=VECTOR('',#11744,1.005);
#3399=VECTOR('',#11751,1.5);
#3400=VECTOR('',#11764,1.005);
#3401=VECTOR('',#11771,1.3);
#3402=VECTOR('',#11788,1.);
#3403=VECTOR('',#11791,0.34);
#3404=VECTOR('',#11796,1.);
#3405=VECTOR('',#11801,1.);
#3406=VECTOR('',#11804,1.);
#3407=VECTOR('',#11805,1.);
#3408=VECTOR('',#11808,1.);
#3409=VECTOR('',#11813,1.);
#3410=VECTOR('',#11814,1.);
#3411=VECTOR('',#11815,1.);
#3412=VECTOR('',#11822,1.);
#3413=VECTOR('',#11823,1.);
#3414=VECTOR('',#11824,1.);
#3415=VECTOR('',#11827,1.);
#3416=VECTOR('',#11836,1.);
#3417=VECTOR('',#11837,1.);
#3418=VECTOR('',#11842,1.);
#3419=VECTOR('',#11851,4.);
#3420=VECTOR('',#11854,1.6);
#3421=VECTOR('',#11867,0.165);
#3422=VECTOR('',#11882,0.5);
#3423=VECTOR('',#11887,0.4);
#3424=VECTOR('',#11898,0.505);
#3425=VECTOR('',#11905,0.7);
#3426=VECTOR('',#11918,0.505);
#3427=VECTOR('',#11925,0.7);
#3428=VECTOR('',#11938,0.225);
#3429=VECTOR('',#11945,0.8);
#3430=VECTOR('',#11956,1.);
#3431=VECTOR('',#11957,1.);
#3432=VECTOR('',#11958,1.);
#3433=VECTOR('',#11959,1.);
#3434=VECTOR('',#11960,1.);
#3435=VECTOR('',#11961,1.);
#3436=VECTOR('',#11962,1.);
#3437=VECTOR('',#11963,1.);
#3438=VECTOR('',#11966,1.);
#3439=VECTOR('',#11967,1.);
#3440=VECTOR('',#11968,1.);
#3441=VECTOR('',#11971,1.);
#3442=VECTOR('',#11972,1.);
#3443=VECTOR('',#11975,1.);
#3444=VECTOR('',#11976,1.);
#3445=VECTOR('',#11979,1.);
#3446=VECTOR('',#11980,1.);
#3447=VECTOR('',#11983,1.);
#3448=VECTOR('',#11984,1.);
#3449=VECTOR('',#11985,1.);
#3450=VECTOR('',#11986,1.);
#3451=VECTOR('',#11989,1.);
#3452=VECTOR('',#11992,1.);
#3453=VECTOR('',#11995,1.);
#3454=VECTOR('',#12002,1.);
#3455=VECTOR('',#12003,1.);
#3456=VECTOR('',#12004,1.);
#3457=VECTOR('',#12005,1.);
#3458=VECTOR('',#12008,1.);
#3459=VECTOR('',#12009,1.);
#3460=VECTOR('',#12010,1.);
#3461=VECTOR('',#12013,1.);
#3462=VECTOR('',#12014,1.);
#3463=VECTOR('',#12015,1.);
#3464=VECTOR('',#12018,1.);
#3465=VECTOR('',#12019,1.);
#3466=VECTOR('',#12020,1.);
#3467=VECTOR('',#12023,1.);
#3468=VECTOR('',#12024,1.);
#3469=VECTOR('',#12025,1.);
#3470=VECTOR('',#12028,1.);
#3471=VECTOR('',#12029,1.);
#3472=VECTOR('',#12040,0.235);
#3473=VECTOR('',#12045,0.25);
#3474=VECTOR('',#12050,0.2125);
#3475=VECTOR('',#12061,1.5);
#3476=VECTOR('',#12068,1.5);
#3477=VECTOR('',#12073,1.);
#3478=VECTOR('',#12076,1.);
#3479=VECTOR('',#12081,1.);
#3480=VECTOR('',#12084,1.);
#3481=VECTOR('',#12087,1.);
#3482=VECTOR('',#12088,1.);
#3483=VECTOR('',#12091,1.);
#3484=VECTOR('',#12096,1.);
#3485=VECTOR('',#12105,1.1);
#3486=VECTOR('',#12112,2.);
#3487=VECTOR('',#12125,1.1);
#3488=VECTOR('',#12132,2.);
#3489=VECTOR('',#12145,1.1);
#3490=VECTOR('',#12152,2.);
#3491=VECTOR('',#12165,1.1);
#3492=VECTOR('',#12172,2.);
#3493=VECTOR('',#12197,0.976185);
#3494=VECTOR('',#12204,0.5);
#3495=VECTOR('',#12209,0.53);
#3496=VECTOR('',#12218,0.976185);
#3497=VECTOR('',#12225,0.53);
#3498=VECTOR('',#12244,1.023815);
#3499=VECTOR('',#12255,1.47);
#3500=VECTOR('',#12260,1.5);
#3501=VECTOR('',#12265,1.47);
#3502=VECTOR('',#12270,1.023815);
#3503=VECTOR('',#12321,1.019052);
#3504=VECTOR('',#12398,0.980948);
#3505=VECTOR('',#12427,1.013815);
#3506=VECTOR('',#12434,0.991185);
#3507=VECTOR('',#12445,1.013815);
#3508=VECTOR('',#12452,0.991185);
#3509=VECTOR('',#12485,0.210000000000001);
#3510=VECTOR('',#12494,0.210000000000001);
#3511=VECTOR('',#12501,1.);
#3512=VECTOR('',#12502,1.);
#3513=VECTOR('',#12503,1.);
#3514=VECTOR('',#12504,1.);
#3515=VECTOR('',#12507,1.);
#3516=VECTOR('',#12508,1.);
#3517=VECTOR('',#12509,1.);
#3518=VECTOR('',#12510,1.);
#3519=VECTOR('',#12513,1.);
#3520=VECTOR('',#12514,1.);
#3521=VECTOR('',#12517,1.);
#3522=VECTOR('',#12522,0.5);
#3523=VECTOR('',#12527,1.);
#3524=VECTOR('',#12528,1.);
#3525=VECTOR('',#12529,1.);
#3526=VECTOR('',#12530,1.);
#3527=VECTOR('',#12533,1.);
#3528=VECTOR('',#12534,1.);
#3529=VECTOR('',#12535,1.);
#3530=VECTOR('',#12538,1.);
#3531=VECTOR('',#12539,1.);
#3532=VECTOR('',#12540,1.);
#3533=VECTOR('',#12543,1.);
#3534=VECTOR('',#12546,1.);
#3535=VECTOR('',#12551,0.275);
#3536=VECTOR('',#12558,0.275);
#3537=VECTOR('',#12565,0.275);
#3538=VECTOR('',#12572,0.275);
#3539=VECTOR('',#12577,1.);
#3540=VECTOR('',#12578,1.);
#3541=VECTOR('',#12579,1.);
#3542=VECTOR('',#12580,1.);
#3543=VECTOR('',#12583,1.);
#3544=VECTOR('',#12584,1.);
#3545=VECTOR('',#12585,1.);
#3546=VECTOR('',#12588,1.);
#3547=VECTOR('',#12589,1.);
#3548=VECTOR('',#12590,1.);
#3549=VECTOR('',#12591,1.);
#3550=VECTOR('',#12594,1.);
#3551=VECTOR('',#12595,1.);
#3552=VECTOR('',#12606,0.275);
#3553=VECTOR('',#12613,0.275);
#3554=VECTOR('',#12618,1.);
#3555=VECTOR('',#12619,1.);
#3556=VECTOR('',#12620,1.);
#3557=VECTOR('',#12621,1.);
#3558=VECTOR('',#12624,1.);
#3559=VECTOR('',#12625,1.);
#3560=VECTOR('',#12626,1.);
#3561=VECTOR('',#12629,1.);
#3562=VECTOR('',#12630,1.);
#3563=VECTOR('',#12631,1.);
#3564=VECTOR('',#12634,1.);
#3565=VECTOR('',#12635,1.);
#3566=VECTOR('',#12646,0.164999999999999);
#3567=VECTOR('',#12659,0.800000000000001);
#3568=VECTOR('',#12668,0.5);
#3569=VECTOR('',#12677,0.505000000000001);
#3570=VECTOR('',#12684,0.699999999999999);
#3571=VECTOR('',#12697,0.505000000000001);
#3572=VECTOR('',#12704,0.699999999999999);
#3573=VECTOR('',#12717,0.225);
#3574=VECTOR('',#12724,0.800000000000001);
#3575=VECTOR('',#12737,1.);
#3576=VECTOR('',#12742,1.);
#3577=VECTOR('',#12745,0.21);
#3578=VECTOR('',#12750,1.);
#3579=VECTOR('',#12753,1.);
#3580=VECTOR('',#12758,1.);
#3581=VECTOR('',#12761,0.21);
#3582=VECTOR('',#12766,1.);
#3583=VECTOR('',#12769,1.);
#3584=VECTOR('',#12774,1.);
#3585=VECTOR('',#12777,0.21);
#3586=VECTOR('',#12782,1.);
#3587=VECTOR('',#12785,1.);
#3588=VECTOR('',#12790,1.);
#3589=VECTOR('',#12793,0.21);
#3590=VECTOR('',#12798,1.);
#3591=VECTOR('',#12801,1.);
#3592=VECTOR('',#12802,1.);
#3593=VECTOR('',#12803,1.);
#3594=VECTOR('',#12804,1.);
#3595=VECTOR('',#12805,1.);
#3596=VECTOR('',#12806,1.);
#3597=VECTOR('',#12809,1.);
#3598=VECTOR('',#12810,1.);
#3599=VECTOR('',#12811,1.);
#3600=VECTOR('',#12812,1.);
#3601=VECTOR('',#12813,1.);
#3602=VECTOR('',#12814,1.);
#3603=VECTOR('',#12817,1.);
#3604=VECTOR('',#12818,1.);
#3605=VECTOR('',#12819,1.);
#3606=VECTOR('',#12820,1.);
#3607=VECTOR('',#12821,1.);
#3608=VECTOR('',#12822,1.);
#3609=VECTOR('',#12823,1.);
#3610=VECTOR('',#12824,1.);
#3611=VECTOR('',#12825,1.);
#3612=VECTOR('',#12826,1.);
#3613=VECTOR('',#12829,1.);
#3614=VECTOR('',#12830,1.);
#3615=VECTOR('',#12833,1.);
#3616=VECTOR('',#12834,1.);
#3617=VECTOR('',#12837,1.);
#3618=VECTOR('',#12838,1.);
#3619=VECTOR('',#12841,1.);
#3620=VECTOR('',#12842,1.);
#3621=VECTOR('',#12845,1.);
#3622=VECTOR('',#12848,1.);
#3623=VECTOR('',#12849,1.);
#3624=VECTOR('',#12852,1.);
#3625=VECTOR('',#12853,1.);
#3626=VECTOR('',#12856,1.);
#3627=VECTOR('',#12857,1.);
#3628=VECTOR('',#12860,1.);
#3629=VECTOR('',#12861,1.);
#3630=VECTOR('',#12864,1.);
#3631=VECTOR('',#12871,1.);
#3632=VECTOR('',#12872,1.);
#3633=VECTOR('',#12873,1.);
#3634=VECTOR('',#12874,1.);
#3635=VECTOR('',#12877,1.);
#3636=VECTOR('',#12878,1.);
#3637=VECTOR('',#12879,1.);
#3638=VECTOR('',#12882,1.);
#3639=VECTOR('',#12883,1.);
#3640=VECTOR('',#12884,1.);
#3641=VECTOR('',#12887,1.);
#3642=VECTOR('',#12888,1.);
#3643=VECTOR('',#12889,1.);
#3644=VECTOR('',#12892,1.);
#3645=VECTOR('',#12893,1.);
#3646=VECTOR('',#12894,1.);
#3647=VECTOR('',#12897,1.);
#3648=VECTOR('',#12898,1.);
#3649=VECTOR('',#12899,1.);
#3650=VECTOR('',#12902,1.);
#3651=VECTOR('',#12903,1.);
#3652=VECTOR('',#12904,1.);
#3653=VECTOR('',#12907,1.);
#3654=VECTOR('',#12908,1.);
#3655=VECTOR('',#12917,1.);
#3656=VECTOR('',#12918,1.);
#3657=VECTOR('',#12919,1.);
#3658=VECTOR('',#12920,1.);
#3659=VECTOR('',#12923,1.);
#3660=VECTOR('',#12924,1.);
#3661=VECTOR('',#12925,1.);
#3662=VECTOR('',#12928,1.);
#3663=VECTOR('',#12929,1.);
#3664=VECTOR('',#12930,1.);
#3665=VECTOR('',#12933,1.);
#3666=VECTOR('',#12934,1.);
#3667=VECTOR('',#12935,1.);
#3668=VECTOR('',#12938,1.);
#3669=VECTOR('',#12939,1.);
#3670=VECTOR('',#12940,1.);
#3671=VECTOR('',#12943,1.);
#3672=VECTOR('',#12944,1.);
#3673=VECTOR('',#12945,1.);
#3674=VECTOR('',#12948,1.);
#3675=VECTOR('',#12949,1.);
#3676=VECTOR('',#12950,1.);
#3677=VECTOR('',#12953,1.);
#3678=VECTOR('',#12954,1.);
#3679=VECTOR('',#12969,1.);
#3680=VECTOR('',#12970,1.);
#3681=VECTOR('',#12971,1.);
#3682=VECTOR('',#12972,1.);
#3683=VECTOR('',#12975,1.);
#3684=VECTOR('',#12976,1.);
#3685=VECTOR('',#12977,1.);
#3686=VECTOR('',#12980,1.);
#3687=VECTOR('',#12981,1.);
#3688=VECTOR('',#12982,1.);
#3689=VECTOR('',#12985,1.);
#3690=VECTOR('',#12986,1.);
#3691=VECTOR('',#12987,1.);
#3692=VECTOR('',#12990,1.);
#3693=VECTOR('',#12991,1.);
#3694=VECTOR('',#12992,1.);
#3695=VECTOR('',#12995,1.);
#3696=VECTOR('',#12996,1.);
#3697=VECTOR('',#13013,0.4);
#3698=VECTOR('',#13018,0.425);
#3699=VECTOR('',#13023,0.41);
#3700=VECTOR('',#13032,0.26);
#3701=VECTOR('',#13035,0.25);
#3702=VECTOR('',#13042,0.275);
#3703=VECTOR('',#13047,0.265);
#3704=VECTOR('',#13056,0.5);
#3705=VECTOR('',#13071,0.4);
#3706=VECTOR('',#13076,0.425);
#3707=VECTOR('',#13081,0.41);
#3708=VECTOR('',#13090,0.26);
#3709=VECTOR('',#13095,0.25);
#3710=VECTOR('',#13100,0.225);
#3711=VECTOR('',#13105,1.);
#3712=VECTOR('',#13106,1.);
#3713=VECTOR('',#13107,1.);
#3714=VECTOR('',#13108,1.);
#3715=VECTOR('',#13111,1.);
#3716=VECTOR('',#13112,1.);
#3717=VECTOR('',#13113,1.);
#3718=VECTOR('',#13116,1.);
#3719=VECTOR('',#13117,1.);
#3720=VECTOR('',#13118,1.);
#3721=VECTOR('',#13121,1.);
#3722=VECTOR('',#13122,1.);
#3723=VECTOR('',#13123,1.);
#3724=VECTOR('',#13126,1.);
#3725=VECTOR('',#13127,1.);
#3726=VECTOR('',#13128,1.);
#3727=VECTOR('',#13131,1.);
#3728=VECTOR('',#13132,1.);
#3729=VECTOR('',#13215,1.);
#3730=VECTOR('',#13216,1.);
#3731=VECTOR('',#13217,1.);
#3732=VECTOR('',#13218,1.);
#3733=VECTOR('',#13221,1.);
#3734=VECTOR('',#13222,1.);
#3735=VECTOR('',#13223,1.);
#3736=VECTOR('',#13226,1.);
#3737=VECTOR('',#13227,1.);
#3738=VECTOR('',#13228,1.);
#3739=VECTOR('',#13231,1.);
#3740=VECTOR('',#13232,1.);
#3741=VECTOR('',#13233,1.);
#3742=VECTOR('',#13236,1.);
#3743=VECTOR('',#13237,1.);
#3744=VECTOR('',#13238,1.);
#3745=VECTOR('',#13241,1.);
#3746=VECTOR('',#13242,1.);
#3747=VECTOR('',#13259,0.325);
#3748=VECTOR('',#13264,0.35);
#3749=VECTOR('',#13269,0.335);
#3750=VECTOR('',#13278,0.21);
#3751=VECTOR('',#13281,0.2);
#3752=CIRCLE('',#9497,0.210000000000001);
#3753=CIRCLE('',#9498,0.210000000000001);
#3754=CIRCLE('',#9500,0.21);
#3755=CIRCLE('',#9501,0.21);
#3756=CIRCLE('',#9503,0.21);
#3757=CIRCLE('',#9504,0.21);
#3758=CIRCLE('',#9506,0.210000000000001);
#3759=CIRCLE('',#9507,0.210000000000001);
#3760=CIRCLE('',#9509,0.21);
#3761=CIRCLE('',#9510,0.21);
#3762=CIRCLE('',#9512,0.21);
#3763=CIRCLE('',#9513,0.21);
#3764=CIRCLE('',#9515,0.21);
#3765=CIRCLE('',#9516,0.21);
#3766=CIRCLE('',#9518,0.21);
#3767=CIRCLE('',#9519,0.21);
#3768=CIRCLE('',#9521,0.21);
#3769=CIRCLE('',#9522,0.21);
#3770=CIRCLE('',#9524,0.21);
#3771=CIRCLE('',#9525,0.21);
#3772=CIRCLE('',#9527,0.21);
#3773=CIRCLE('',#9528,0.21);
#3774=CIRCLE('',#9530,0.21);
#3775=CIRCLE('',#9531,0.21);
#3776=CIRCLE('',#9540,0.34);
#3777=CIRCLE('',#9541,0.34);
#3778=CIRCLE('',#9544,0.34);
#3779=CIRCLE('',#9545,0.34);
#3780=CIRCLE('',#9548,0.5);
#3781=CIRCLE('',#9549,0.5);
#3782=CIRCLE('',#9551,0.275);
#3783=CIRCLE('',#9553,0.5);
#3784=CIRCLE('',#9554,0.5);
#3785=CIRCLE('',#9556,0.275);
#3786=CIRCLE('',#9558,0.5);
#3787=CIRCLE('',#9559,0.5);
#3788=CIRCLE('',#9561,0.275);
#3789=CIRCLE('',#9563,0.5);
#3790=CIRCLE('',#9564,0.5);
#3791=CIRCLE('',#9566,0.275);
#3792=CIRCLE('',#9568,0.275);
#3793=CIRCLE('',#9570,0.275);
#3794=CIRCLE('',#9572,0.275);
#3795=CIRCLE('',#9574,0.275);
#3796=CIRCLE('',#9583,0.425);
#3797=CIRCLE('',#9584,0.425);
#3798=CIRCLE('',#9586,0.645);
#3799=CIRCLE('',#9587,0.645);
#3800=CIRCLE('',#9592,0.425);
#3801=CIRCLE('',#9593,0.425);
#3802=CIRCLE('',#9595,0.645);
#3803=CIRCLE('',#9596,0.645);
#3804=CIRCLE('',#9601,0.34);
#3805=CIRCLE('',#9602,0.34);
#3806=CIRCLE('',#9605,0.34);
#3807=CIRCLE('',#9606,0.34);
#3808=CIRCLE('',#9609,0.5);
#3809=CIRCLE('',#9610,0.5);
#3810=CIRCLE('',#9612,0.275);
#3811=CIRCLE('',#9614,0.5);
#3812=CIRCLE('',#9615,0.5);
#3813=CIRCLE('',#9617,0.275);
#3814=CIRCLE('',#9619,0.5);
#3815=CIRCLE('',#9620,0.5);
#3816=CIRCLE('',#9622,0.275);
#3817=CIRCLE('',#9624,0.5);
#3818=CIRCLE('',#9625,0.5);
#3819=CIRCLE('',#9627,0.275);
#3820=CIRCLE('',#9629,0.275);
#3821=CIRCLE('',#9631,0.275);
#3822=CIRCLE('',#9633,0.275);
#3823=CIRCLE('',#9635,0.275);
#3824=CIRCLE('',#9644,0.425);
#3825=CIRCLE('',#9645,0.425);
#3826=CIRCLE('',#9647,0.645);
#3827=CIRCLE('',#9648,0.645);
#3828=CIRCLE('',#9653,0.425);
#3829=CIRCLE('',#9654,0.425);
#3830=CIRCLE('',#9656,0.645);
#3831=CIRCLE('',#9657,0.645);
#3832=CIRCLE('',#9662,0.164999999999999);
#3833=CIRCLE('',#9663,0.164999999999999);
#3834=CIRCLE('',#9666,0.164999999999999);
#3835=CIRCLE('',#9667,0.164999999999999);
#3836=CIRCLE('',#9670,0.165);
#3837=CIRCLE('',#9671,0.165);
#3838=CIRCLE('',#9674,0.164999999999999);
#3839=CIRCLE('',#9675,0.164999999999999);
#3840=CIRCLE('',#9678,0.5);
#3841=CIRCLE('',#9679,0.5);
#3842=CIRCLE('',#9681,0.274999999999999);
#3843=CIRCLE('',#9683,0.5);
#3844=CIRCLE('',#9684,0.5);
#3845=CIRCLE('',#9686,0.275);
#3846=CIRCLE('',#9688,0.5);
#3847=CIRCLE('',#9689,0.5);
#3848=CIRCLE('',#9691,0.275);
#3849=CIRCLE('',#9693,0.5);
#3850=CIRCLE('',#9694,0.5);
#3851=CIRCLE('',#9696,0.274999999999999);
#3852=CIRCLE('',#9698,0.274999999999999);
#3853=CIRCLE('',#9700,0.275);
#3854=CIRCLE('',#9702,0.275);
#3855=CIRCLE('',#9704,0.274999999999999);
#3856=CIRCLE('',#9728,2.05);
#3857=CIRCLE('',#9729,2.05);
#3858=CIRCLE('',#9731,2.05);
#3859=CIRCLE('',#9732,2.05);
#3860=CIRCLE('',#9734,2.35);
#3861=CIRCLE('',#9736,2.8);
#3862=CIRCLE('',#9738,2.8);
#3863=CIRCLE('',#9740,2.8);
#3864=CIRCLE('',#9743,2.8);
#3865=CIRCLE('',#9746,0.65);
#3866=CIRCLE('',#9747,0.65);
#3867=CIRCLE('',#9749,2.8);
#3868=CIRCLE('',#9750,2.8);
#3869=CIRCLE('',#9759,0.65);
#3870=CIRCLE('',#9761,0.65);
#3871=CIRCLE('',#9769,1.8);
#3872=CIRCLE('',#9770,1.8);
#3873=CIRCLE('',#9772,2.19089023002066);
#3874=CIRCLE('',#9774,2.35);
#3875=CIRCLE('',#9775,2.19089023002066);
#3876=CIRCLE('',#9780,1.65);
#3877=CIRCLE('',#9781,1.65);
#3878=CIRCLE('',#9787,1.);
#3879=CIRCLE('',#9789,1.75);
#3880=CIRCLE('',#9791,1.75);
#3881=CIRCLE('',#9793,1.);
#3882=CIRCLE('',#9799,0.42);
#3883=CIRCLE('',#9800,0.42);
#3884=CIRCLE('',#9802,0.8);
#3885=CIRCLE('',#9803,0.8);
#3886=CIRCLE('',#9816,0.3933);
#3887=CIRCLE('',#9818,0.6);
#3888=CIRCLE('',#9820,0.65);
#3889=CIRCLE('',#9822,0.65);
#3890=CIRCLE('',#9824,0.62);
#3891=CIRCLE('',#9826,0.42);
#3892=CIRCLE('',#9828,0.3933);
#3893=CIRCLE('',#9832,0.375);
#3894=CIRCLE('',#9833,0.375);
#3895=CIRCLE('',#9835,0.225);
#3896=CIRCLE('',#9837,0.375);
#3897=CIRCLE('',#9838,0.375);
#3898=CIRCLE('',#9840,0.225);
#3899=CIRCLE('',#9842,0.375);
#3900=CIRCLE('',#9843,0.375);
#3901=CIRCLE('',#9845,0.225);
#3902=CIRCLE('',#9847,0.375);
#3903=CIRCLE('',#9848,0.375);
#3904=CIRCLE('',#9850,0.225000000000001);
#3905=CIRCLE('',#9852,0.225);
#3906=CIRCLE('',#9854,0.225);
#3907=CIRCLE('',#9856,0.225);
#3908=CIRCLE('',#9858,0.225000000000001);
#3909=CIRCLE('',#9875,0.3);
#3910=CIRCLE('',#9877,0.35);
#3911=CIRCLE('',#9879,0.35);
#3912=CIRCLE('',#9881,0.32);
#3913=CIRCLE('',#9883,0.22);
#3914=CIRCLE('',#9885,0.1954);
#3915=CIRCLE('',#9887,0.1954);
#3916=CIRCLE('',#9889,0.16);
#3917=CIRCLE('',#9903,1.);
#3918=CIRCLE('',#9907,1.);
#3919=CIRCLE('',#9908,1.);
#3920=CIRCLE('',#9909,1.);
#3921=CIRCLE('',#9914,0.21);
#3922=CIRCLE('',#9916,0.21);
#3923=CIRCLE('',#9917,0.21);
#3924=CIRCLE('',#9920,1.005);
#3925=CIRCLE('',#9921,1.005);
#3926=CIRCLE('',#9923,1.5);
#3927=CIRCLE('',#9924,1.5);
#3928=CIRCLE('',#9929,0.21);
#3929=CIRCLE('',#9931,0.21);
#3930=CIRCLE('',#9932,0.21);
#3931=CIRCLE('',#9935,1.005);
#3932=CIRCLE('',#9936,1.005);
#3933=CIRCLE('',#9938,1.5);
#3934=CIRCLE('',#9939,1.5);
#3935=CIRCLE('',#9944,1.005);
#3936=CIRCLE('',#9945,1.005);
#3937=CIRCLE('',#9947,1.3);
#3938=CIRCLE('',#9948,1.3);
#3939=CIRCLE('',#9953,1.);
#3940=CIRCLE('',#9954,0.34);
#3941=CIRCLE('',#9956,0.34);
#3942=CIRCLE('',#9957,0.34);
#3943=CIRCLE('',#9958,0.34);
#3944=CIRCLE('',#9960,1.);
#3945=CIRCLE('',#9961,1.);
#3946=CIRCLE('',#9962,1.);
#3947=CIRCLE('',#9963,1.);
#3948=CIRCLE('',#9966,4.);
#3949=CIRCLE('',#9970,0.21);
#3950=CIRCLE('',#9972,0.21);
#3951=CIRCLE('',#9976,4.);
#3952=CIRCLE('',#9977,1.6);
#3953=CIRCLE('',#9980,1.6);
#3954=CIRCLE('',#9981,1.6);
#3955=CIRCLE('',#9985,0.165);
#3956=CIRCLE('',#9986,0.165);
#3957=CIRCLE('',#9989,0.5);
#3958=CIRCLE('',#9990,0.4);
#3959=CIRCLE('',#9992,0.5);
#3960=CIRCLE('',#9995,0.4);
#3961=CIRCLE('',#9999,0.505);
#3962=CIRCLE('',#10000,0.505);
#3963=CIRCLE('',#10002,0.7);
#3964=CIRCLE('',#10003,0.7);
#3965=CIRCLE('',#10008,0.505);
#3966=CIRCLE('',#10009,0.505);
#3967=CIRCLE('',#10011,0.7);
#3968=CIRCLE('',#10012,0.7);
#3969=CIRCLE('',#10017,0.225);
#3970=CIRCLE('',#10018,0.225);
#3971=CIRCLE('',#10020,0.8);
#3972=CIRCLE('',#10021,0.8);
#3973=CIRCLE('',#10044,0.22);
#3974=CIRCLE('',#10046,0.24505);
#3975=CIRCLE('',#10048,0.24505);
#3976=CIRCLE('',#10050,0.175);
#3977=CIRCLE('',#10055,1.5);
#3978=CIRCLE('',#10056,1.5);
#3979=CIRCLE('',#10058,1.5);
#3980=CIRCLE('',#10059,1.5);
#3981=CIRCLE('',#10061,2.);
#3982=CIRCLE('',#10062,2.);
#3983=CIRCLE('',#10064,2.);
#3984=CIRCLE('',#10067,2.);
#3985=CIRCLE('',#10072,1.1);
#3986=CIRCLE('',#10073,1.1);
#3987=CIRCLE('',#10075,2.);
#3988=CIRCLE('',#10076,2.);
#3989=CIRCLE('',#10081,1.1);
#3990=CIRCLE('',#10082,1.1);
#3991=CIRCLE('',#10084,2.);
#3992=CIRCLE('',#10085,2.);
#3993=CIRCLE('',#10090,1.1);
#3994=CIRCLE('',#10091,1.1);
#3995=CIRCLE('',#10093,2.);
#3996=CIRCLE('',#10094,2.);
#3997=CIRCLE('',#10099,1.1);
#3998=CIRCLE('',#10100,1.1);
#3999=CIRCLE('',#10102,2.);
#4000=CIRCLE('',#10103,2.);
#4001=CIRCLE('',#10109,0.976185);
#4002=CIRCLE('',#10110,0.976185);
#4003=CIRCLE('',#10111,0.247676);
#4004=CIRCLE('',#10112,0.976185);
#4005=CIRCLE('',#10113,0.976185);
#4006=CIRCLE('',#10115,0.976185);
#4007=CIRCLE('',#10117,0.5);
#4008=CIRCLE('',#10118,0.5);
#4009=CIRCLE('',#10120,0.56);
#4010=CIRCLE('',#10123,0.976185);
#4011=CIRCLE('',#10125,0.56);
#4012=CIRCLE('',#10129,1.023815);
#4013=CIRCLE('',#10130,1.023815);
#4014=CIRCLE('',#10131,0.247676);
#4015=CIRCLE('',#10132,1.023815);
#4016=CIRCLE('',#10133,1.023815);
#4017=CIRCLE('',#10135,1.023815);
#4018=CIRCLE('',#10137,1.44);
#4019=CIRCLE('',#10138,1.023815);
#4020=CIRCLE('',#10140,1.5);
#4021=CIRCLE('',#10142,1.5);
#4022=CIRCLE('',#10144,1.44);
#4023=CIRCLE('',#10149,0.23815);
#4024=CIRCLE('',#10151,0.23815);
#4025=CIRCLE('',#10153,0.23815);
#4026=CIRCLE('',#10155,0.23815);
#4027=CIRCLE('',#10157,0.23815);
#4028=CIRCLE('',#10159,0.23815);
#4029=CIRCLE('',#10161,0.23815);
#4030=CIRCLE('',#10163,0.23815);
#4031=CIRCLE('',#10166,0.243053047864041);
#4032=CIRCLE('',#10167,0.243053047864041);
#4033=CIRCLE('',#10169,1.019052);
#4034=CIRCLE('',#10170,1.019052);
#4035=CIRCLE('',#10171,1.019052);
#4036=CIRCLE('',#10172,1.019052);
#4037=CIRCLE('',#10173,1.019052);
#4038=CIRCLE('',#10174,1.019052);
#4039=CIRCLE('',#10175,1.019052);
#4040=CIRCLE('',#10176,1.019052);
#4041=CIRCLE('',#10177,1.019052);
#4042=CIRCLE('',#10179,0.980948);
#4043=CIRCLE('',#10180,0.243053047864041);
#4044=CIRCLE('',#10182,0.243053047864041);
#4045=CIRCLE('',#10184,0.980948);
#4046=CIRCLE('',#10185,0.243053047864041);
#4047=CIRCLE('',#10187,0.243053047864041);
#4048=CIRCLE('',#10189,0.980948);
#4049=CIRCLE('',#10190,0.243053047864041);
#4050=CIRCLE('',#10192,0.243053047864041);
#4051=CIRCLE('',#10194,0.980948);
#4052=CIRCLE('',#10195,0.243053047864041);
#4053=CIRCLE('',#10197,0.243053047864041);
#4054=CIRCLE('',#10199,0.980948);
#4055=CIRCLE('',#10200,0.243053047864041);
#4056=CIRCLE('',#10202,0.243053047864041);
#4057=CIRCLE('',#10204,0.980948);
#4058=CIRCLE('',#10205,0.243053047864041);
#4059=CIRCLE('',#10207,0.243053047864041);
#4060=CIRCLE('',#10209,0.980948);
#4061=CIRCLE('',#10210,0.980948);
#4062=CIRCLE('',#10211,0.980948);
#4063=CIRCLE('',#10213,0.243053047864041);
#4064=CIRCLE('',#10215,0.243053047864041);
#4065=CIRCLE('',#10220,1.013815);
#4066=CIRCLE('',#10221,0.991185);
#4067=CIRCLE('',#10223,1.013815);
#4068=CIRCLE('',#10225,0.991185);
#4069=CIRCLE('',#10228,1.013815);
#4070=CIRCLE('',#10229,0.991185);
#4071=CIRCLE('',#10231,1.013815);
#4072=CIRCLE('',#10233,0.991185);
#4073=CIRCLE('',#10250,0.210000000000001);
#4074=CIRCLE('',#10251,0.210000000000001);
#4075=CIRCLE('',#10254,0.210000000000001);
#4076=CIRCLE('',#10255,0.210000000000001);
#4077=CIRCLE('',#10262,0.5);
#4078=CIRCLE('',#10263,0.5);
#4079=CIRCLE('',#10270,0.275);
#4080=CIRCLE('',#10271,0.275);
#4081=CIRCLE('',#10273,0.275);
#4082=CIRCLE('',#10274,0.275);
#4083=CIRCLE('',#10276,0.275);
#4084=CIRCLE('',#10277,0.275);
#4085=CIRCLE('',#10279,0.275);
#4086=CIRCLE('',#10280,0.275);
#4087=CIRCLE('',#10289,0.275);
#4088=CIRCLE('',#10290,0.275);
#4089=CIRCLE('',#10292,0.275);
#4090=CIRCLE('',#10293,0.275);
#4091=CIRCLE('',#10302,0.164999999999999);
#4092=CIRCLE('',#10303,0.164999999999999);
#4093=CIRCLE('',#10306,0.800000000000001);
#4094=CIRCLE('',#10307,0.5);
#4095=CIRCLE('',#10309,0.800000000000001);
#4096=CIRCLE('',#10312,0.5);
#4097=CIRCLE('',#10316,0.505000000000001);
#4098=CIRCLE('',#10317,0.505000000000001);
#4099=CIRCLE('',#10319,0.699999999999999);
#4100=CIRCLE('',#10320,0.699999999999999);
#4101=CIRCLE('',#10325,0.505000000000001);
#4102=CIRCLE('',#10326,0.505000000000001);
#4103=CIRCLE('',#10328,0.699999999999999);
#4104=CIRCLE('',#10329,0.699999999999999);
#4105=CIRCLE('',#10334,0.225);
#4106=CIRCLE('',#10335,0.225);
#4107=CIRCLE('',#10337,0.800000000000001);
#4108=CIRCLE('',#10338,0.800000000000001);
#4109=CIRCLE('',#10344,0.21);
#4110=CIRCLE('',#10346,0.21);
#4111=CIRCLE('',#10347,0.21);
#4112=CIRCLE('',#10348,0.21);
#4113=CIRCLE('',#10350,0.21);
#4114=CIRCLE('',#10352,0.21);
#4115=CIRCLE('',#10353,0.21);
#4116=CIRCLE('',#10354,0.21);
#4117=CIRCLE('',#10356,0.21);
#4118=CIRCLE('',#10358,0.21);
#4119=CIRCLE('',#10359,0.21);
#4120=CIRCLE('',#10360,0.21);
#4121=CIRCLE('',#10362,0.21);
#4122=CIRCLE('',#10364,0.21);
#4123=CIRCLE('',#10365,0.21);
#4124=CIRCLE('',#10366,0.21);
#4125=CIRCLE('',#10416,0.24505);
#4126=CIRCLE('',#10418,0.375);
#4127=CIRCLE('',#10420,0.425);
#4128=CIRCLE('',#10422,0.425);
#4129=CIRCLE('',#10424,0.395);
#4130=CIRCLE('',#10426,0.27);
#4131=CIRCLE('',#10428,0.24505);
#4132=CIRCLE('',#10432,0.285);
#4133=CIRCLE('',#10433,0.265);
#4134=CIRCLE('',#10435,0.265);
#4135=CIRCLE('',#10437,0.5);
#4136=CIRCLE('',#10439,0.5);
#4137=CIRCLE('',#10443,0.375);
#4138=CIRCLE('',#10445,0.425);
#4139=CIRCLE('',#10447,0.425);
#4140=CIRCLE('',#10449,0.395);
#4141=CIRCLE('',#10451,0.27);
#4142=CIRCLE('',#10453,0.24505);
#4143=CIRCLE('',#10455,0.24505);
#4144=CIRCLE('',#10457,0.2);
#4145=CIRCLE('',#10514,0.1954);
#4146=CIRCLE('',#10516,0.3);
#4147=CIRCLE('',#10518,0.35);
#4148=CIRCLE('',#10520,0.35);
#4149=CIRCLE('',#10522,0.32);
#4150=CIRCLE('',#10524,0.22);
#4151=CIRCLE('',#10526,0.1954);
#4152=VERTEX_POINT('',#13362);
#4153=VERTEX_POINT('',#13364);
#4154=VERTEX_POINT('',#13368);
#4155=VERTEX_POINT('',#13370);
#4156=VERTEX_POINT('',#13374);
#4157=VERTEX_POINT('',#13376);
#4158=VERTEX_POINT('',#13380);
#4159=VERTEX_POINT('',#13382);
#4160=VERTEX_POINT('',#13386);
#4161=VERTEX_POINT('',#13388);
#4162=VERTEX_POINT('',#13392);
#4163=VERTEX_POINT('',#13394);
#4164=VERTEX_POINT('',#13398);
#4165=VERTEX_POINT('',#13400);
#4166=VERTEX_POINT('',#13404);
#4167=VERTEX_POINT('',#13406);
#4168=VERTEX_POINT('',#13410);
#4169=VERTEX_POINT('',#13412);
#4170=VERTEX_POINT('',#13416);
#4171=VERTEX_POINT('',#13418);
#4172=VERTEX_POINT('',#13422);
#4173=VERTEX_POINT('',#13424);
#4174=VERTEX_POINT('',#13428);
#4175=VERTEX_POINT('',#13430);
#4176=VERTEX_POINT('',#13434);
#4177=VERTEX_POINT('',#13435);
#4178=VERTEX_POINT('',#13437);
#4179=VERTEX_POINT('',#13439);
#4180=VERTEX_POINT('',#13443);
#4181=VERTEX_POINT('',#13445);
#4182=VERTEX_POINT('',#13449);
#4183=VERTEX_POINT('',#13451);
#4184=VERTEX_POINT('',#13461);
#4185=VERTEX_POINT('',#13463);
#4186=VERTEX_POINT('',#13468);
#4187=VERTEX_POINT('',#13470);
#4188=VERTEX_POINT('',#13475);
#4189=VERTEX_POINT('',#13477);
#4190=VERTEX_POINT('',#13481);
#4191=VERTEX_POINT('',#13484);
#4192=VERTEX_POINT('',#13486);
#4193=VERTEX_POINT('',#13490);
#4194=VERTEX_POINT('',#13493);
#4195=VERTEX_POINT('',#13495);
#4196=VERTEX_POINT('',#13499);
#4197=VERTEX_POINT('',#13502);
#4198=VERTEX_POINT('',#13504);
#4199=VERTEX_POINT('',#13508);
#4200=VERTEX_POINT('',#13511);
#4201=VERTEX_POINT('',#13515);
#4202=VERTEX_POINT('',#13519);
#4203=VERTEX_POINT('',#13523);
#4204=VERTEX_POINT('',#13527);
#4205=VERTEX_POINT('',#13528);
#4206=VERTEX_POINT('',#13530);
#4207=VERTEX_POINT('',#13532);
#4208=VERTEX_POINT('',#13536);
#4209=VERTEX_POINT('',#13538);
#4210=VERTEX_POINT('',#13542);
#4211=VERTEX_POINT('',#13544);
#4212=VERTEX_POINT('',#13554);
#4213=VERTEX_POINT('',#13556);
#4214=VERTEX_POINT('',#13560);
#4215=VERTEX_POINT('',#13562);
#4216=VERTEX_POINT('',#13569);
#4217=VERTEX_POINT('',#13571);
#4218=VERTEX_POINT('',#13575);
#4219=VERTEX_POINT('',#13577);
#4220=VERTEX_POINT('',#13584);
#4221=VERTEX_POINT('',#13586);
#4222=VERTEX_POINT('',#13591);
#4223=VERTEX_POINT('',#13593);
#4224=VERTEX_POINT('',#13598);
#4225=VERTEX_POINT('',#13600);
#4226=VERTEX_POINT('',#13604);
#4227=VERTEX_POINT('',#13607);
#4228=VERTEX_POINT('',#13609);
#4229=VERTEX_POINT('',#13613);
#4230=VERTEX_POINT('',#13616);
#4231=VERTEX_POINT('',#13618);
#4232=VERTEX_POINT('',#13622);
#4233=VERTEX_POINT('',#13625);
#4234=VERTEX_POINT('',#13627);
#4235=VERTEX_POINT('',#13631);
#4236=VERTEX_POINT('',#13634);
#4237=VERTEX_POINT('',#13638);
#4238=VERTEX_POINT('',#13642);
#4239=VERTEX_POINT('',#13646);
#4240=VERTEX_POINT('',#13650);
#4241=VERTEX_POINT('',#13651);
#4242=VERTEX_POINT('',#13653);
#4243=VERTEX_POINT('',#13655);
#4244=VERTEX_POINT('',#13659);
#4245=VERTEX_POINT('',#13661);
#4246=VERTEX_POINT('',#13665);
#4247=VERTEX_POINT('',#13667);
#4248=VERTEX_POINT('',#13677);
#4249=VERTEX_POINT('',#13679);
#4250=VERTEX_POINT('',#13683);
#4251=VERTEX_POINT('',#13685);
#4252=VERTEX_POINT('',#13692);
#4253=VERTEX_POINT('',#13694);
#4254=VERTEX_POINT('',#13698);
#4255=VERTEX_POINT('',#13700);
#4256=VERTEX_POINT('',#13707);
#4257=VERTEX_POINT('',#13709);
#4258=VERTEX_POINT('',#13714);
#4259=VERTEX_POINT('',#13716);
#4260=VERTEX_POINT('',#13721);
#4261=VERTEX_POINT('',#13723);
#4262=VERTEX_POINT('',#13728);
#4263=VERTEX_POINT('',#13730);
#4264=VERTEX_POINT('',#13735);
#4265=VERTEX_POINT('',#13737);
#4266=VERTEX_POINT('',#13741);
#4267=VERTEX_POINT('',#13744);
#4268=VERTEX_POINT('',#13746);
#4269=VERTEX_POINT('',#13750);
#4270=VERTEX_POINT('',#13753);
#4271=VERTEX_POINT('',#13755);
#4272=VERTEX_POINT('',#13759);
#4273=VERTEX_POINT('',#13762);
#4274=VERTEX_POINT('',#13764);
#4275=VERTEX_POINT('',#13768);
#4276=VERTEX_POINT('',#13771);
#4277=VERTEX_POINT('',#13775);
#4278=VERTEX_POINT('',#13779);
#4279=VERTEX_POINT('',#13783);
#4280=VERTEX_POINT('',#13787);
#4281=VERTEX_POINT('',#13788);
#4282=VERTEX_POINT('',#13790);
#4283=VERTEX_POINT('',#13792);
#4284=VERTEX_POINT('',#13796);
#4285=VERTEX_POINT('',#13798);
#4286=VERTEX_POINT('',#13802);
#4287=VERTEX_POINT('',#13804);
#4288=VERTEX_POINT('',#13814);
#4289=VERTEX_POINT('',#13815);
#4290=VERTEX_POINT('',#13817);
#4291=VERTEX_POINT('',#13819);
#4292=VERTEX_POINT('',#13823);
#4293=VERTEX_POINT('',#13825);
#4294=VERTEX_POINT('',#13829);
#4295=VERTEX_POINT('',#13831);
#4296=VERTEX_POINT('',#13841);
#4297=VERTEX_POINT('',#13842);
#4298=VERTEX_POINT('',#13844);
#4299=VERTEX_POINT('',#13846);
#4300=VERTEX_POINT('',#13850);
#4301=VERTEX_POINT('',#13852);
#4302=VERTEX_POINT('',#13856);
#4303=VERTEX_POINT('',#13858);
#4304=VERTEX_POINT('',#13869);
#4305=VERTEX_POINT('',#13871);
#4306=VERTEX_POINT('',#13875);
#4307=VERTEX_POINT('',#13877);
#4308=VERTEX_POINT('',#13881);
#4309=VERTEX_POINT('',#13882);
#4310=VERTEX_POINT('',#13885);
#4311=VERTEX_POINT('',#13886);
#4312=VERTEX_POINT('',#13888);
#4313=VERTEX_POINT('',#13892);
#4314=VERTEX_POINT('',#13893);
#4315=VERTEX_POINT('',#13895);
#4316=VERTEX_POINT('',#13899);
#4317=VERTEX_POINT('',#13900);
#4318=VERTEX_POINT('',#13902);
#4319=VERTEX_POINT('',#13909);
#4320=VERTEX_POINT('',#13910);
#4321=VERTEX_POINT('',#13912);
#4322=VERTEX_POINT('',#13919);
#4323=VERTEX_POINT('',#13920);
#4324=VERTEX_POINT('',#13922);
#4325=VERTEX_POINT('',#13924);
#4326=VERTEX_POINT('',#13927);
#4327=VERTEX_POINT('',#13929);
#4328=VERTEX_POINT('',#13931);
#4329=VERTEX_POINT('',#13933);
#4330=VERTEX_POINT('',#13936);
#4331=VERTEX_POINT('',#13938);
#4332=VERTEX_POINT('',#13947);
#4333=VERTEX_POINT('',#13948);
#4334=VERTEX_POINT('',#13950);
#4335=VERTEX_POINT('',#13952);
#4336=VERTEX_POINT('',#13956);
#4337=VERTEX_POINT('',#13958);
#4338=VERTEX_POINT('',#13962);
#4339=VERTEX_POINT('',#13964);
#4340=VERTEX_POINT('',#13972);
#4341=VERTEX_POINT('',#13976);
#4342=VERTEX_POINT('',#13980);
#4343=VERTEX_POINT('',#13981);
#4344=VERTEX_POINT('',#13986);
#4345=VERTEX_POINT('',#13990);
#4346=VERTEX_POINT('',#13998);
#4347=VERTEX_POINT('',#14000);
#4348=VERTEX_POINT('',#14004);
#4349=VERTEX_POINT('',#14007);
#4350=VERTEX_POINT('',#14008);
#4351=VERTEX_POINT('',#14010);
#4352=VERTEX_POINT('',#14014);
#4353=VERTEX_POINT('',#14015);
#4354=VERTEX_POINT('',#14026);
#4355=VERTEX_POINT('',#14055);
#4356=VERTEX_POINT('',#14092);
#4357=VERTEX_POINT('',#14127);
#4358=VERTEX_POINT('',#14129);
#4359=VERTEX_POINT('',#14140);
#4360=VERTEX_POINT('',#14170);
#4361=VERTEX_POINT('',#14172);
#4362=VERTEX_POINT('',#14175);
#4363=VERTEX_POINT('',#14176);
#4364=VERTEX_POINT('',#14195);
#4365=VERTEX_POINT('',#14216);
#4366=VERTEX_POINT('',#14217);
#4367=VERTEX_POINT('',#14236);
#4368=VERTEX_POINT('',#14257);
#4369=VERTEX_POINT('',#14258);
#4370=VERTEX_POINT('',#14277);
#4371=VERTEX_POINT('',#14298);
#4372=VERTEX_POINT('',#14299);
#4373=VERTEX_POINT('',#14318);
#4374=VERTEX_POINT('',#14340);
#4375=VERTEX_POINT('',#14377);
#4376=VERTEX_POINT('',#14414);
#4377=VERTEX_POINT('',#14451);
#4378=VERTEX_POINT('',#14488);
#4379=VERTEX_POINT('',#14491);
#4380=VERTEX_POINT('',#14494);
#4381=VERTEX_POINT('',#14498);
#4382=VERTEX_POINT('',#14506);
#4383=VERTEX_POINT('',#14508);
#4384=VERTEX_POINT('',#14512);
#4385=VERTEX_POINT('',#14514);
#4386=VERTEX_POINT('',#14521);
#4387=VERTEX_POINT('',#14522);
#4388=VERTEX_POINT('',#14524);
#4389=VERTEX_POINT('',#14526);
#4390=VERTEX_POINT('',#14530);
#4391=VERTEX_POINT('',#14532);
#4392=VERTEX_POINT('',#14536);
#4393=VERTEX_POINT('',#14538);
#4394=VERTEX_POINT('',#14542);
#4395=VERTEX_POINT('',#14544);
#4396=VERTEX_POINT('',#14548);
#4397=VERTEX_POINT('',#14550);
#4398=VERTEX_POINT('',#14559);
#4399=VERTEX_POINT('',#14562);
#4400=VERTEX_POINT('',#14565);
#4401=VERTEX_POINT('',#14569);
#4402=VERTEX_POINT('',#14573);
#4403=VERTEX_POINT('',#14577);
#4404=VERTEX_POINT('',#14580);
#4405=VERTEX_POINT('',#14587);
#4406=VERTEX_POINT('',#14589);
#4407=VERTEX_POINT('',#14593);
#4408=VERTEX_POINT('',#14596);
#4409=VERTEX_POINT('',#14598);
#4410=VERTEX_POINT('',#14602);
#4411=VERTEX_POINT('',#14605);
#4412=VERTEX_POINT('',#14607);
#4413=VERTEX_POINT('',#14611);
#4414=VERTEX_POINT('',#14614);
#4415=VERTEX_POINT('',#14616);
#4416=VERTEX_POINT('',#14620);
#4417=VERTEX_POINT('',#14623);
#4418=VERTEX_POINT('',#14627);
#4419=VERTEX_POINT('',#14631);
#4420=VERTEX_POINT('',#14635);
#4421=VERTEX_POINT('',#14639);
#4422=VERTEX_POINT('',#14640);
#4423=VERTEX_POINT('',#14642);
#4424=VERTEX_POINT('',#14644);
#4425=VERTEX_POINT('',#14648);
#4426=VERTEX_POINT('',#14650);
#4427=VERTEX_POINT('',#14654);
#4428=VERTEX_POINT('',#14656);
#4429=VERTEX_POINT('',#14660);
#4430=VERTEX_POINT('',#14662);
#4431=VERTEX_POINT('',#14666);
#4432=VERTEX_POINT('',#14668);
#4433=VERTEX_POINT('',#14672);
#4434=VERTEX_POINT('',#14674);
#4435=VERTEX_POINT('',#14678);
#4436=VERTEX_POINT('',#14680);
#4437=VERTEX_POINT('',#14684);
#4438=VERTEX_POINT('',#14686);
#4439=VERTEX_POINT('',#14690);
#4440=VERTEX_POINT('',#14692);
#4441=VERTEX_POINT('',#14696);
#4442=VERTEX_POINT('',#14698);
#4443=VERTEX_POINT('',#14702);
#4444=VERTEX_POINT('',#14704);
#4445=VERTEX_POINT('',#14714);
#4446=VERTEX_POINT('',#14717);
#4447=VERTEX_POINT('',#14721);
#4448=VERTEX_POINT('',#14725);
#4449=VERTEX_POINT('',#14729);
#4450=VERTEX_POINT('',#14732);
#4451=VERTEX_POINT('',#14736);
#4452=VERTEX_POINT('',#14740);
#4453=VERTEX_POINT('',#14745);
#4454=VERTEX_POINT('',#14746);
#4455=VERTEX_POINT('',#14748);
#4456=VERTEX_POINT('',#14750);
#4457=VERTEX_POINT('',#14754);
#4458=VERTEX_POINT('',#14756);
#4459=VERTEX_POINT('',#14760);
#4460=VERTEX_POINT('',#14762);
#4461=VERTEX_POINT('',#14766);
#4462=VERTEX_POINT('',#14768);
#4463=VERTEX_POINT('',#14772);
#4464=VERTEX_POINT('',#14774);
#4465=VERTEX_POINT('',#14785);
#4466=VERTEX_POINT('',#14786);
#4467=VERTEX_POINT('',#14788);
#4468=VERTEX_POINT('',#14790);
#4469=VERTEX_POINT('',#14794);
#4470=VERTEX_POINT('',#14796);
#4471=VERTEX_POINT('',#14800);
#4472=VERTEX_POINT('',#14802);
#4473=VERTEX_POINT('',#14808);
#4474=VERTEX_POINT('',#14810);
#4475=VERTEX_POINT('',#14818);
#4476=VERTEX_POINT('',#14819);
#4477=VERTEX_POINT('',#14823);
#4478=VERTEX_POINT('',#14838);
#4479=VERTEX_POINT('',#14840);
#4480=VERTEX_POINT('',#14842);
#4481=VERTEX_POINT('',#14879);
#4482=VERTEX_POINT('',#14898);
#4483=VERTEX_POINT('',#14900);
#4484=VERTEX_POINT('',#14904);
#4485=VERTEX_POINT('',#14906);
#4486=VERTEX_POINT('',#14913);
#4487=VERTEX_POINT('',#14914);
#4488=VERTEX_POINT('',#14918);
#4489=VERTEX_POINT('',#14933);
#4490=VERTEX_POINT('',#14935);
#4491=VERTEX_POINT('',#14937);
#4492=VERTEX_POINT('',#14974);
#4493=VERTEX_POINT('',#14993);
#4494=VERTEX_POINT('',#14995);
#4495=VERTEX_POINT('',#14999);
#4496=VERTEX_POINT('',#15001);
#4497=VERTEX_POINT('',#15008);
#4498=VERTEX_POINT('',#15010);
#4499=VERTEX_POINT('',#15014);
#4500=VERTEX_POINT('',#15016);
#4501=VERTEX_POINT('',#15023);
#4502=VERTEX_POINT('',#15024);
#4503=VERTEX_POINT('',#15028);
#4504=VERTEX_POINT('',#15030);
#4505=VERTEX_POINT('',#15032);
#4506=VERTEX_POINT('',#15035);
#4507=VERTEX_POINT('',#15039);
#4508=VERTEX_POINT('',#15041);
#4509=VERTEX_POINT('',#15043);
#4510=VERTEX_POINT('',#15045);
#4511=VERTEX_POINT('',#15052);
#4512=VERTEX_POINT('',#15054);
#4513=VERTEX_POINT('',#15065);
#4514=VERTEX_POINT('',#15067);
#4515=VERTEX_POINT('',#15074);
#4516=VERTEX_POINT('',#15076);
#4517=VERTEX_POINT('',#15080);
#4518=VERTEX_POINT('',#15082);
#4519=VERTEX_POINT('',#15086);
#4520=VERTEX_POINT('',#15089);
#4521=VERTEX_POINT('',#15091);
#4522=VERTEX_POINT('',#15100);
#4523=VERTEX_POINT('',#15102);
#4524=VERTEX_POINT('',#15143);
#4525=VERTEX_POINT('',#15145);
#4526=VERTEX_POINT('',#15150);
#4527=VERTEX_POINT('',#15157);
#4528=VERTEX_POINT('',#15159);
#4529=VERTEX_POINT('',#15164);
#4530=VERTEX_POINT('',#15166);
#4531=VERTEX_POINT('',#15169);
#4532=VERTEX_POINT('',#15174);
#4533=VERTEX_POINT('',#15180);
#4534=VERTEX_POINT('',#15182);
#4535=VERTEX_POINT('',#15186);
#4536=VERTEX_POINT('',#15188);
#4537=VERTEX_POINT('',#15195);
#4538=VERTEX_POINT('',#15197);
#4539=VERTEX_POINT('',#15201);
#4540=VERTEX_POINT('',#15203);
#4541=VERTEX_POINT('',#15210);
#4542=VERTEX_POINT('',#15212);
#4543=VERTEX_POINT('',#15216);
#4544=VERTEX_POINT('',#15218);
#4545=VERTEX_POINT('',#15225);
#4546=VERTEX_POINT('',#15226);
#4547=VERTEX_POINT('',#15228);
#4548=VERTEX_POINT('',#15230);
#4549=VERTEX_POINT('',#15232);
#4550=VERTEX_POINT('',#15234);
#4551=VERTEX_POINT('',#15236);
#4552=VERTEX_POINT('',#15238);
#4553=VERTEX_POINT('',#15242);
#4554=VERTEX_POINT('',#15244);
#4555=VERTEX_POINT('',#15248);
#4556=VERTEX_POINT('',#15252);
#4557=VERTEX_POINT('',#15256);
#4558=VERTEX_POINT('',#15260);
#4559=VERTEX_POINT('',#15261);
#4560=VERTEX_POINT('',#15264);
#4561=VERTEX_POINT('',#15276);
#4562=VERTEX_POINT('',#15277);
#4563=VERTEX_POINT('',#15279);
#4564=VERTEX_POINT('',#15281);
#4565=VERTEX_POINT('',#15285);
#4566=VERTEX_POINT('',#15287);
#4567=VERTEX_POINT('',#15291);
#4568=VERTEX_POINT('',#15293);
#4569=VERTEX_POINT('',#15297);
#4570=VERTEX_POINT('',#15299);
#4571=VERTEX_POINT('',#15303);
#4572=VERTEX_POINT('',#15305);
#4573=VERTEX_POINT('',#15313);
#4574=VERTEX_POINT('',#15316);
#4575=VERTEX_POINT('',#15320);
#4576=VERTEX_POINT('',#15324);
#4577=VERTEX_POINT('',#15331);
#4578=VERTEX_POINT('',#15333);
#4579=VERTEX_POINT('',#15337);
#4580=VERTEX_POINT('',#15339);
#4581=VERTEX_POINT('',#15343);
#4582=VERTEX_POINT('',#15344);
#4583=VERTEX_POINT('',#15346);
#4584=VERTEX_POINT('',#15348);
#4585=VERTEX_POINT('',#15352);
#4586=VERTEX_POINT('',#15354);
#4587=VERTEX_POINT('',#15358);
#4588=VERTEX_POINT('',#15362);
#4589=VERTEX_POINT('',#15370);
#4590=VERTEX_POINT('',#15372);
#4591=VERTEX_POINT('',#15376);
#4592=VERTEX_POINT('',#15378);
#4593=VERTEX_POINT('',#15385);
#4594=VERTEX_POINT('',#15387);
#4595=VERTEX_POINT('',#15391);
#4596=VERTEX_POINT('',#15393);
#4597=VERTEX_POINT('',#15400);
#4598=VERTEX_POINT('',#15402);
#4599=VERTEX_POINT('',#15406);
#4600=VERTEX_POINT('',#15408);
#4601=VERTEX_POINT('',#15415);
#4602=VERTEX_POINT('',#15417);
#4603=VERTEX_POINT('',#15421);
#4604=VERTEX_POINT('',#15423);
#4605=VERTEX_POINT('',#15431);
#4606=VERTEX_POINT('',#15432);
#4607=VERTEX_POINT('',#15435);
#4608=VERTEX_POINT('',#15437);
#4609=VERTEX_POINT('',#15441);
#4610=VERTEX_POINT('',#15445);
#4611=VERTEX_POINT('',#15447);
#4612=VERTEX_POINT('',#15451);
#4613=VERTEX_POINT('',#15456);
#4614=VERTEX_POINT('',#15460);
#4615=VERTEX_POINT('',#15466);
#4616=VERTEX_POINT('',#15467);
#4617=VERTEX_POINT('',#15470);
#4618=VERTEX_POINT('',#15472);
#4619=VERTEX_POINT('',#15476);
#4620=VERTEX_POINT('',#15480);
#4621=VERTEX_POINT('',#15482);
#4622=VERTEX_POINT('',#15485);
#4623=VERTEX_POINT('',#15489);
#4624=VERTEX_POINT('',#15493);
#4625=VERTEX_POINT('',#15501);
#4626=VERTEX_POINT('',#15502);
#4627=VERTEX_POINT('',#15505);
#4628=VERTEX_POINT('',#15506);
#4629=VERTEX_POINT('',#15509);
#4630=VERTEX_POINT('',#15510);
#4631=VERTEX_POINT('',#15513);
#4632=VERTEX_POINT('',#15514);
#4633=VERTEX_POINT('',#15517);
#4634=VERTEX_POINT('',#15518);
#4635=VERTEX_POINT('',#15521);
#4636=VERTEX_POINT('',#15522);
#4637=VERTEX_POINT('',#15525);
#4638=VERTEX_POINT('',#15526);
#4639=VERTEX_POINT('',#15529);
#4640=VERTEX_POINT('',#15530);
#4641=VERTEX_POINT('',#15534);
#4642=VERTEX_POINT('',#15535);
#4643=VERTEX_POINT('',#15558);
#4644=VERTEX_POINT('',#15560);
#4645=VERTEX_POINT('',#15585);
#4646=VERTEX_POINT('',#15587);
#4647=VERTEX_POINT('',#15610);
#4648=VERTEX_POINT('',#15612);
#4649=VERTEX_POINT('',#15635);
#4650=VERTEX_POINT('',#15637);
#4651=VERTEX_POINT('',#15650);
#4652=VERTEX_POINT('',#15653);
#4653=VERTEX_POINT('',#15666);
#4654=VERTEX_POINT('',#15668);
#4655=VERTEX_POINT('',#15691);
#4656=VERTEX_POINT('',#15693);
#4657=VERTEX_POINT('',#15716);
#4658=VERTEX_POINT('',#15718);
#4659=VERTEX_POINT('',#15741);
#4660=VERTEX_POINT('',#15743);
#4661=VERTEX_POINT('',#15768);
#4662=VERTEX_POINT('',#15772);
#4663=VERTEX_POINT('',#15797);
#4664=VERTEX_POINT('',#15801);
#4665=VERTEX_POINT('',#15826);
#4666=VERTEX_POINT('',#15830);
#4667=VERTEX_POINT('',#15831);
#4668=VERTEX_POINT('',#15858);
#4669=VERTEX_POINT('',#15862);
#4670=VERTEX_POINT('',#15887);
#4671=VERTEX_POINT('',#15891);
#4672=VERTEX_POINT('',#15916);
#4673=VERTEX_POINT('',#15920);
#4674=VERTEX_POINT('',#15945);
#4675=VERTEX_POINT('',#15948);
#4676=VERTEX_POINT('',#15950);
#4677=VERTEX_POINT('',#15982);
#4678=VERTEX_POINT('',#15984);
#4679=VERTEX_POINT('',#15987);
#4680=VERTEX_POINT('',#15991);
#4681=VERTEX_POINT('',#15996);
#4682=VERTEX_POINT('',#15998);
#4683=VERTEX_POINT('',#16001);
#4684=VERTEX_POINT('',#16005);
#4685=VERTEX_POINT('',#16024);
#4686=VERTEX_POINT('',#16026);
#4687=VERTEX_POINT('',#16031);
#4688=VERTEX_POINT('',#16033);
#4689=VERTEX_POINT('',#16038);
#4690=VERTEX_POINT('',#16039);
#4691=VERTEX_POINT('',#16041);
#4692=VERTEX_POINT('',#16043);
#4693=VERTEX_POINT('',#16047);
#4694=VERTEX_POINT('',#16048);
#4695=VERTEX_POINT('',#16050);
#4696=VERTEX_POINT('',#16052);
#4697=VERTEX_POINT('',#16061);
#4698=VERTEX_POINT('',#16063);
#4699=VERTEX_POINT('',#16067);
#4700=VERTEX_POINT('',#16068);
#4701=VERTEX_POINT('',#16070);
#4702=VERTEX_POINT('',#16072);
#4703=VERTEX_POINT('',#16076);
#4704=VERTEX_POINT('',#16078);
#4705=VERTEX_POINT('',#16082);
#4706=VERTEX_POINT('',#16084);
#4707=VERTEX_POINT('',#16092);
#4708=VERTEX_POINT('',#16094);
#4709=VERTEX_POINT('',#16098);
#4710=VERTEX_POINT('',#16100);
#4711=VERTEX_POINT('',#16104);
#4712=VERTEX_POINT('',#16106);
#4713=VERTEX_POINT('',#16110);
#4714=VERTEX_POINT('',#16112);
#4715=VERTEX_POINT('',#16116);
#4716=VERTEX_POINT('',#16117);
#4717=VERTEX_POINT('',#16119);
#4718=VERTEX_POINT('',#16121);
#4719=VERTEX_POINT('',#16125);
#4720=VERTEX_POINT('',#16127);
#4721=VERTEX_POINT('',#16131);
#4722=VERTEX_POINT('',#16134);
#4723=VERTEX_POINT('',#16144);
#4724=VERTEX_POINT('',#16146);
#4725=VERTEX_POINT('',#16150);
#4726=VERTEX_POINT('',#16152);
#4727=VERTEX_POINT('',#16156);
#4728=VERTEX_POINT('',#16157);
#4729=VERTEX_POINT('',#16159);
#4730=VERTEX_POINT('',#16161);
#4731=VERTEX_POINT('',#16165);
#4732=VERTEX_POINT('',#16167);
#4733=VERTEX_POINT('',#16171);
#4734=VERTEX_POINT('',#16173);
#4735=VERTEX_POINT('',#16183);
#4736=VERTEX_POINT('',#16185);
#4737=VERTEX_POINT('',#16190);
#4738=VERTEX_POINT('',#16192);
#4739=VERTEX_POINT('',#16195);
#4740=VERTEX_POINT('',#16200);
#4741=VERTEX_POINT('',#16206);
#4742=VERTEX_POINT('',#16208);
#4743=VERTEX_POINT('',#16212);
#4744=VERTEX_POINT('',#16214);
#4745=VERTEX_POINT('',#16221);
#4746=VERTEX_POINT('',#16223);
#4747=VERTEX_POINT('',#16227);
#4748=VERTEX_POINT('',#16229);
#4749=VERTEX_POINT('',#16236);
#4750=VERTEX_POINT('',#16238);
#4751=VERTEX_POINT('',#16242);
#4752=VERTEX_POINT('',#16244);
#4753=VERTEX_POINT('',#16252);
#4754=VERTEX_POINT('',#16253);
#4755=VERTEX_POINT('',#16257);
#4756=VERTEX_POINT('',#16259);
#4757=VERTEX_POINT('',#16261);
#4758=VERTEX_POINT('',#16264);
#4759=VERTEX_POINT('',#16268);
#4760=VERTEX_POINT('',#16269);
#4761=VERTEX_POINT('',#16273);
#4762=VERTEX_POINT('',#16275);
#4763=VERTEX_POINT('',#16277);
#4764=VERTEX_POINT('',#16280);
#4765=VERTEX_POINT('',#16284);
#4766=VERTEX_POINT('',#16285);
#4767=VERTEX_POINT('',#16289);
#4768=VERTEX_POINT('',#16291);
#4769=VERTEX_POINT('',#16293);
#4770=VERTEX_POINT('',#16296);
#4771=VERTEX_POINT('',#16300);
#4772=VERTEX_POINT('',#16301);
#4773=VERTEX_POINT('',#16305);
#4774=VERTEX_POINT('',#16307);
#4775=VERTEX_POINT('',#16309);
#4776=VERTEX_POINT('',#16312);
#4777=VERTEX_POINT('',#16317);
#4778=VERTEX_POINT('',#16319);
#4779=VERTEX_POINT('',#16321);
#4780=VERTEX_POINT('',#16323);
#4781=VERTEX_POINT('',#16328);
#4782=VERTEX_POINT('',#16330);
#4783=VERTEX_POINT('',#16332);
#4784=VERTEX_POINT('',#16334);
#4785=VERTEX_POINT('',#16338);
#4786=VERTEX_POINT('',#16340);
#4787=VERTEX_POINT('',#16342);
#4788=VERTEX_POINT('',#16344);
#4789=VERTEX_POINT('',#16347);
#4790=VERTEX_POINT('',#16349);
#4791=VERTEX_POINT('',#16351);
#4792=VERTEX_POINT('',#16353);
#4793=VERTEX_POINT('',#16357);
#4794=VERTEX_POINT('',#16361);
#4795=VERTEX_POINT('',#16365);
#4796=VERTEX_POINT('',#16369);
#4797=VERTEX_POINT('',#16375);
#4798=VERTEX_POINT('',#16379);
#4799=VERTEX_POINT('',#16383);
#4800=VERTEX_POINT('',#16387);
#4801=VERTEX_POINT('',#16395);
#4802=VERTEX_POINT('',#16396);
#4803=VERTEX_POINT('',#16398);
#4804=VERTEX_POINT('',#16400);
#4805=VERTEX_POINT('',#16404);
#4806=VERTEX_POINT('',#16406);
#4807=VERTEX_POINT('',#16410);
#4808=VERTEX_POINT('',#16412);
#4809=VERTEX_POINT('',#16416);
#4810=VERTEX_POINT('',#16418);
#4811=VERTEX_POINT('',#16422);
#4812=VERTEX_POINT('',#16424);
#4813=VERTEX_POINT('',#16428);
#4814=VERTEX_POINT('',#16430);
#4815=VERTEX_POINT('',#16434);
#4816=VERTEX_POINT('',#16436);
#4817=VERTEX_POINT('',#16446);
#4818=VERTEX_POINT('',#16447);
#4819=VERTEX_POINT('',#16449);
#4820=VERTEX_POINT('',#16451);
#4821=VERTEX_POINT('',#16455);
#4822=VERTEX_POINT('',#16457);
#4823=VERTEX_POINT('',#16461);
#4824=VERTEX_POINT('',#16463);
#4825=VERTEX_POINT('',#16467);
#4826=VERTEX_POINT('',#16469);
#4827=VERTEX_POINT('',#16473);
#4828=VERTEX_POINT('',#16475);
#4829=VERTEX_POINT('',#16479);
#4830=VERTEX_POINT('',#16481);
#4831=VERTEX_POINT('',#16485);
#4832=VERTEX_POINT('',#16487);
#4833=VERTEX_POINT('',#16500);
#4834=VERTEX_POINT('',#16501);
#4835=VERTEX_POINT('',#16503);
#4836=VERTEX_POINT('',#16505);
#4837=VERTEX_POINT('',#16509);
#4838=VERTEX_POINT('',#16511);
#4839=VERTEX_POINT('',#16515);
#4840=VERTEX_POINT('',#16517);
#4841=VERTEX_POINT('',#16521);
#4842=VERTEX_POINT('',#16523);
#4843=VERTEX_POINT('',#16527);
#4844=VERTEX_POINT('',#16529);
#4845=VERTEX_POINT('',#16538);
#4846=VERTEX_POINT('',#16541);
#4847=VERTEX_POINT('',#16544);
#4848=VERTEX_POINT('',#16548);
#4849=VERTEX_POINT('',#16552);
#4850=VERTEX_POINT('',#16556);
#4851=VERTEX_POINT('',#16559);
#4852=VERTEX_POINT('',#16566);
#4853=VERTEX_POINT('',#16568);
#4854=VERTEX_POINT('',#16572);
#4855=VERTEX_POINT('',#16576);
#4856=VERTEX_POINT('',#16579);
#4857=VERTEX_POINT('',#16585);
#4858=VERTEX_POINT('',#16588);
#4859=VERTEX_POINT('',#16592);
#4860=VERTEX_POINT('',#16596);
#4861=VERTEX_POINT('',#16600);
#4862=VERTEX_POINT('',#16603);
#4863=VERTEX_POINT('',#16607);
#4864=VERTEX_POINT('',#16611);
#4865=VERTEX_POINT('',#16616);
#4866=VERTEX_POINT('',#16617);
#4867=VERTEX_POINT('',#16619);
#4868=VERTEX_POINT('',#16621);
#4869=VERTEX_POINT('',#16625);
#4870=VERTEX_POINT('',#16627);
#4871=VERTEX_POINT('',#16631);
#4872=VERTEX_POINT('',#16633);
#4873=VERTEX_POINT('',#16637);
#4874=VERTEX_POINT('',#16639);
#4875=VERTEX_POINT('',#16643);
#4876=VERTEX_POINT('',#16645);
#4877=VERTEX_POINT('',#16692);
#4878=VERTEX_POINT('',#16693);
#4879=VERTEX_POINT('',#16695);
#4880=VERTEX_POINT('',#16697);
#4881=VERTEX_POINT('',#16701);
#4882=VERTEX_POINT('',#16703);
#4883=VERTEX_POINT('',#16707);
#4884=VERTEX_POINT('',#16709);
#4885=VERTEX_POINT('',#16713);
#4886=VERTEX_POINT('',#16715);
#4887=VERTEX_POINT('',#16719);
#4888=VERTEX_POINT('',#16721);
#4889=VERTEX_POINT('',#16730);
#4890=VERTEX_POINT('',#16733);
#4891=VERTEX_POINT('',#16736);
#4892=VERTEX_POINT('',#16740);
#4893=VERTEX_POINT('',#16744);
#4894=VERTEX_POINT('',#16748);
#4895=VERTEX_POINT('',#16751);
#4896=EDGE_CURVE('',#4152,#4152,#3752,.T.);
#4897=EDGE_CURVE('',#4152,#4153,#2460,.T.);
#4898=EDGE_CURVE('',#4153,#4153,#3753,.T.);
#4899=EDGE_CURVE('',#4154,#4154,#3754,.T.);
#4900=EDGE_CURVE('',#4154,#4155,#2461,.T.);
#4901=EDGE_CURVE('',#4155,#4155,#3755,.T.);
#4902=EDGE_CURVE('',#4156,#4156,#3756,.T.);
#4903=EDGE_CURVE('',#4156,#4157,#2462,.T.);
#4904=EDGE_CURVE('',#4157,#4157,#3757,.T.);
#4905=EDGE_CURVE('',#4158,#4158,#3758,.T.);
#4906=EDGE_CURVE('',#4158,#4159,#2463,.T.);
#4907=EDGE_CURVE('',#4159,#4159,#3759,.T.);
#4908=EDGE_CURVE('',#4160,#4160,#3760,.T.);
#4909=EDGE_CURVE('',#4160,#4161,#2464,.T.);
#4910=EDGE_CURVE('',#4161,#4161,#3761,.T.);
#4911=EDGE_CURVE('',#4162,#4162,#3762,.T.);
#4912=EDGE_CURVE('',#4162,#4163,#2465,.T.);
#4913=EDGE_CURVE('',#4163,#4163,#3763,.T.);
#4914=EDGE_CURVE('',#4164,#4164,#3764,.T.);
#4915=EDGE_CURVE('',#4164,#4165,#2466,.T.);
#4916=EDGE_CURVE('',#4165,#4165,#3765,.T.);
#4917=EDGE_CURVE('',#4166,#4166,#3766,.T.);
#4918=EDGE_CURVE('',#4166,#4167,#2467,.T.);
#4919=EDGE_CURVE('',#4167,#4167,#3767,.T.);
#4920=EDGE_CURVE('',#4168,#4168,#3768,.T.);
#4921=EDGE_CURVE('',#4168,#4169,#2468,.T.);
#4922=EDGE_CURVE('',#4169,#4169,#3769,.T.);
#4923=EDGE_CURVE('',#4170,#4170,#3770,.T.);
#4924=EDGE_CURVE('',#4170,#4171,#2469,.T.);
#4925=EDGE_CURVE('',#4171,#4171,#3771,.T.);
#4926=EDGE_CURVE('',#4172,#4172,#3772,.T.);
#4927=EDGE_CURVE('',#4172,#4173,#2470,.T.);
#4928=EDGE_CURVE('',#4173,#4173,#3773,.T.);
#4929=EDGE_CURVE('',#4174,#4174,#3774,.T.);
#4930=EDGE_CURVE('',#4174,#4175,#2471,.T.);
#4931=EDGE_CURVE('',#4175,#4175,#3775,.T.);
#4932=EDGE_CURVE('',#4176,#4177,#2472,.T.);
#4933=EDGE_CURVE('',#4177,#4178,#2473,.T.);
#4934=EDGE_CURVE('',#4179,#4178,#2474,.T.);
#4935=EDGE_CURVE('',#4176,#4179,#2475,.T.);
#4936=EDGE_CURVE('',#4180,#4176,#2476,.T.);
#4937=EDGE_CURVE('',#4181,#4179,#2477,.T.);
#4938=EDGE_CURVE('',#4180,#4181,#2478,.T.);
#4939=EDGE_CURVE('',#4182,#4180,#2479,.T.);
#4940=EDGE_CURVE('',#4183,#4181,#2480,.T.);
#4941=EDGE_CURVE('',#4182,#4183,#2481,.T.);
#4942=EDGE_CURVE('',#4177,#4182,#2482,.T.);
#4943=EDGE_CURVE('',#4178,#4183,#2483,.T.);
#4944=EDGE_CURVE('',#4184,#4184,#3776,.T.);
#4945=EDGE_CURVE('',#4184,#4185,#2484,.T.);
#4946=EDGE_CURVE('',#4185,#4185,#3777,.T.);
#4947=EDGE_CURVE('',#4186,#4186,#3778,.T.);
#4948=EDGE_CURVE('',#4186,#4187,#2485,.T.);
#4949=EDGE_CURVE('',#4187,#4187,#3779,.T.);
#4950=EDGE_CURVE('',#4188,#4188,#3780,.T.);
#4951=EDGE_CURVE('',#4188,#4189,#2486,.T.);
#4952=EDGE_CURVE('',#4189,#4189,#3781,.T.);
#4953=EDGE_CURVE('',#4190,#4190,#3782,.T.);
#4954=EDGE_CURVE('',#4191,#4191,#3783,.T.);
#4955=EDGE_CURVE('',#4191,#4192,#2487,.T.);
#4956=EDGE_CURVE('',#4192,#4192,#3784,.T.);
#4957=EDGE_CURVE('',#4193,#4193,#3785,.T.);
#4958=EDGE_CURVE('',#4194,#4194,#3786,.T.);
#4959=EDGE_CURVE('',#4194,#4195,#2488,.T.);
#4960=EDGE_CURVE('',#4195,#4195,#3787,.T.);
#4961=EDGE_CURVE('',#4196,#4196,#3788,.T.);
#4962=EDGE_CURVE('',#4197,#4197,#3789,.T.);
#4963=EDGE_CURVE('',#4197,#4198,#2489,.T.);
#4964=EDGE_CURVE('',#4198,#4198,#3790,.T.);
#4965=EDGE_CURVE('',#4199,#4199,#3791,.T.);
#4966=EDGE_CURVE('',#4200,#4200,#3792,.T.);
#4967=EDGE_CURVE('',#4200,#4190,#2490,.T.);
#4968=EDGE_CURVE('',#4201,#4201,#3793,.T.);
#4969=EDGE_CURVE('',#4201,#4193,#2491,.T.);
#4970=EDGE_CURVE('',#4202,#4202,#3794,.T.);
#4971=EDGE_CURVE('',#4202,#4196,#2492,.T.);
#4972=EDGE_CURVE('',#4203,#4203,#3795,.T.);
#4973=EDGE_CURVE('',#4203,#4199,#2493,.T.);
#4974=EDGE_CURVE('',#4204,#4205,#2494,.T.);
#4975=EDGE_CURVE('',#4205,#4206,#2495,.T.);
#4976=EDGE_CURVE('',#4207,#4206,#2496,.T.);
#4977=EDGE_CURVE('',#4204,#4207,#2497,.T.);
#4978=EDGE_CURVE('',#4208,#4204,#2498,.T.);
#4979=EDGE_CURVE('',#4209,#4207,#2499,.T.);
#4980=EDGE_CURVE('',#4208,#4209,#2500,.T.);
#4981=EDGE_CURVE('',#4210,#4208,#2501,.T.);
#4982=EDGE_CURVE('',#4211,#4209,#2502,.T.);
#4983=EDGE_CURVE('',#4210,#4211,#2503,.T.);
#4984=EDGE_CURVE('',#4205,#4210,#2504,.T.);
#4985=EDGE_CURVE('',#4206,#4211,#2505,.T.);
#4986=EDGE_CURVE('',#4212,#4212,#3796,.T.);
#4987=EDGE_CURVE('',#4212,#4213,#2506,.T.);
#4988=EDGE_CURVE('',#4213,#4213,#3797,.T.);
#4989=EDGE_CURVE('',#4214,#4214,#3798,.T.);
#4990=EDGE_CURVE('',#4214,#4215,#2507,.T.);
#4991=EDGE_CURVE('',#4215,#4215,#3799,.T.);
#4992=EDGE_CURVE('',#4216,#4216,#3800,.T.);
#4993=EDGE_CURVE('',#4216,#4217,#2508,.T.);
#4994=EDGE_CURVE('',#4217,#4217,#3801,.T.);
#4995=EDGE_CURVE('',#4218,#4218,#3802,.T.);
#4996=EDGE_CURVE('',#4218,#4219,#2509,.T.);
#4997=EDGE_CURVE('',#4219,#4219,#3803,.T.);
#4998=EDGE_CURVE('',#4220,#4220,#3804,.T.);
#4999=EDGE_CURVE('',#4220,#4221,#2510,.T.);
#5000=EDGE_CURVE('',#4221,#4221,#3805,.T.);
#5001=EDGE_CURVE('',#4222,#4222,#3806,.T.);
#5002=EDGE_CURVE('',#4222,#4223,#2511,.T.);
#5003=EDGE_CURVE('',#4223,#4223,#3807,.T.);
#5004=EDGE_CURVE('',#4224,#4224,#3808,.T.);
#5005=EDGE_CURVE('',#4224,#4225,#2512,.T.);
#5006=EDGE_CURVE('',#4225,#4225,#3809,.T.);
#5007=EDGE_CURVE('',#4226,#4226,#3810,.T.);
#5008=EDGE_CURVE('',#4227,#4227,#3811,.T.);
#5009=EDGE_CURVE('',#4227,#4228,#2513,.T.);
#5010=EDGE_CURVE('',#4228,#4228,#3812,.T.);
#5011=EDGE_CURVE('',#4229,#4229,#3813,.T.);
#5012=EDGE_CURVE('',#4230,#4230,#3814,.T.);
#5013=EDGE_CURVE('',#4230,#4231,#2514,.T.);
#5014=EDGE_CURVE('',#4231,#4231,#3815,.T.);
#5015=EDGE_CURVE('',#4232,#4232,#3816,.T.);
#5016=EDGE_CURVE('',#4233,#4233,#3817,.T.);
#5017=EDGE_CURVE('',#4233,#4234,#2515,.T.);
#5018=EDGE_CURVE('',#4234,#4234,#3818,.T.);
#5019=EDGE_CURVE('',#4235,#4235,#3819,.T.);
#5020=EDGE_CURVE('',#4236,#4236,#3820,.T.);
#5021=EDGE_CURVE('',#4236,#4226,#2516,.T.);
#5022=EDGE_CURVE('',#4237,#4237,#3821,.T.);
#5023=EDGE_CURVE('',#4237,#4229,#2517,.T.);
#5024=EDGE_CURVE('',#4238,#4238,#3822,.T.);
#5025=EDGE_CURVE('',#4238,#4232,#2518,.T.);
#5026=EDGE_CURVE('',#4239,#4239,#3823,.T.);
#5027=EDGE_CURVE('',#4239,#4235,#2519,.T.);
#5028=EDGE_CURVE('',#4240,#4241,#2520,.T.);
#5029=EDGE_CURVE('',#4241,#4242,#2521,.T.);
#5030=EDGE_CURVE('',#4243,#4242,#2522,.T.);
#5031=EDGE_CURVE('',#4240,#4243,#2523,.T.);
#5032=EDGE_CURVE('',#4244,#4240,#2524,.T.);
#5033=EDGE_CURVE('',#4245,#4243,#2525,.T.);
#5034=EDGE_CURVE('',#4244,#4245,#2526,.T.);
#5035=EDGE_CURVE('',#4246,#4244,#2527,.T.);
#5036=EDGE_CURVE('',#4247,#4245,#2528,.T.);
#5037=EDGE_CURVE('',#4246,#4247,#2529,.T.);
#5038=EDGE_CURVE('',#4241,#4246,#2530,.T.);
#5039=EDGE_CURVE('',#4242,#4247,#2531,.T.);
#5040=EDGE_CURVE('',#4248,#4248,#3824,.T.);
#5041=EDGE_CURVE('',#4248,#4249,#2532,.T.);
#5042=EDGE_CURVE('',#4249,#4249,#3825,.T.);
#5043=EDGE_CURVE('',#4250,#4250,#3826,.T.);
#5044=EDGE_CURVE('',#4250,#4251,#2533,.T.);
#5045=EDGE_CURVE('',#4251,#4251,#3827,.T.);
#5046=EDGE_CURVE('',#4252,#4252,#3828,.T.);
#5047=EDGE_CURVE('',#4252,#4253,#2534,.T.);
#5048=EDGE_CURVE('',#4253,#4253,#3829,.T.);
#5049=EDGE_CURVE('',#4254,#4254,#3830,.T.);
#5050=EDGE_CURVE('',#4254,#4255,#2535,.T.);
#5051=EDGE_CURVE('',#4255,#4255,#3831,.T.);
#5052=EDGE_CURVE('',#4256,#4256,#3832,.T.);
#5053=EDGE_CURVE('',#4256,#4257,#2536,.T.);
#5054=EDGE_CURVE('',#4257,#4257,#3833,.T.);
#5055=EDGE_CURVE('',#4258,#4258,#3834,.T.);
#5056=EDGE_CURVE('',#4258,#4259,#2537,.T.);
#5057=EDGE_CURVE('',#4259,#4259,#3835,.T.);
#5058=EDGE_CURVE('',#4260,#4260,#3836,.T.);
#5059=EDGE_CURVE('',#4260,#4261,#2538,.T.);
#5060=EDGE_CURVE('',#4261,#4261,#3837,.T.);
#5061=EDGE_CURVE('',#4262,#4262,#3838,.T.);
#5062=EDGE_CURVE('',#4262,#4263,#2539,.T.);
#5063=EDGE_CURVE('',#4263,#4263,#3839,.T.);
#5064=EDGE_CURVE('',#4264,#4264,#3840,.T.);
#5065=EDGE_CURVE('',#4264,#4265,#2540,.T.);
#5066=EDGE_CURVE('',#4265,#4265,#3841,.T.);
#5067=EDGE_CURVE('',#4266,#4266,#3842,.T.);
#5068=EDGE_CURVE('',#4267,#4267,#3843,.T.);
#5069=EDGE_CURVE('',#4267,#4268,#2541,.T.);
#5070=EDGE_CURVE('',#4268,#4268,#3844,.T.);
#5071=EDGE_CURVE('',#4269,#4269,#3845,.T.);
#5072=EDGE_CURVE('',#4270,#4270,#3846,.T.);
#5073=EDGE_CURVE('',#4270,#4271,#2542,.T.);
#5074=EDGE_CURVE('',#4271,#4271,#3847,.T.);
#5075=EDGE_CURVE('',#4272,#4272,#3848,.T.);
#5076=EDGE_CURVE('',#4273,#4273,#3849,.T.);
#5077=EDGE_CURVE('',#4273,#4274,#2543,.T.);
#5078=EDGE_CURVE('',#4274,#4274,#3850,.T.);
#5079=EDGE_CURVE('',#4275,#4275,#3851,.T.);
#5080=EDGE_CURVE('',#4276,#4276,#3852,.T.);
#5081=EDGE_CURVE('',#4276,#4266,#2544,.T.);
#5082=EDGE_CURVE('',#4277,#4277,#3853,.T.);
#5083=EDGE_CURVE('',#4277,#4269,#2545,.T.);
#5084=EDGE_CURVE('',#4278,#4278,#3854,.T.);
#5085=EDGE_CURVE('',#4278,#4272,#2546,.T.);
#5086=EDGE_CURVE('',#4279,#4279,#3855,.T.);
#5087=EDGE_CURVE('',#4279,#4275,#2547,.T.);
#5088=EDGE_CURVE('',#4280,#4281,#2548,.T.);
#5089=EDGE_CURVE('',#4281,#4282,#2549,.T.);
#5090=EDGE_CURVE('',#4283,#4282,#2550,.T.);
#5091=EDGE_CURVE('',#4280,#4283,#2551,.T.);
#5092=EDGE_CURVE('',#4284,#4280,#2552,.T.);
#5093=EDGE_CURVE('',#4285,#4283,#2553,.T.);
#5094=EDGE_CURVE('',#4284,#4285,#2554,.T.);
#5095=EDGE_CURVE('',#4286,#4284,#2555,.T.);
#5096=EDGE_CURVE('',#4287,#4285,#2556,.T.);
#5097=EDGE_CURVE('',#4286,#4287,#2557,.T.);
#5098=EDGE_CURVE('',#4281,#4286,#2558,.T.);
#5099=EDGE_CURVE('',#4282,#4287,#2559,.T.);
#5100=EDGE_CURVE('',#4288,#4289,#2560,.T.);
#5101=EDGE_CURVE('',#4289,#4290,#2561,.T.);
#5102=EDGE_CURVE('',#4291,#4290,#2562,.T.);
#5103=EDGE_CURVE('',#4288,#4291,#2563,.T.);
#5104=EDGE_CURVE('',#4292,#4288,#2564,.T.);
#5105=EDGE_CURVE('',#4293,#4291,#2565,.T.);
#5106=EDGE_CURVE('',#4292,#4293,#2566,.T.);
#5107=EDGE_CURVE('',#4294,#4292,#2567,.T.);
#5108=EDGE_CURVE('',#4295,#4293,#2568,.T.);
#5109=EDGE_CURVE('',#4294,#4295,#2569,.T.);
#5110=EDGE_CURVE('',#4289,#4294,#2570,.T.);
#5111=EDGE_CURVE('',#4290,#4295,#2571,.T.);
#5112=EDGE_CURVE('',#4296,#4297,#2572,.T.);
#5113=EDGE_CURVE('',#4297,#4298,#2573,.T.);
#5114=EDGE_CURVE('',#4299,#4298,#2574,.T.);
#5115=EDGE_CURVE('',#4296,#4299,#2575,.T.);
#5116=EDGE_CURVE('',#4300,#4296,#2576,.T.);
#5117=EDGE_CURVE('',#4301,#4299,#2577,.T.);
#5118=EDGE_CURVE('',#4300,#4301,#2578,.T.);
#5119=EDGE_CURVE('',#4302,#4300,#2579,.T.);
#5120=EDGE_CURVE('',#4303,#4301,#2580,.T.);
#5121=EDGE_CURVE('',#4302,#4303,#2581,.T.);
#5122=EDGE_CURVE('',#4297,#4302,#2582,.T.);
#5123=EDGE_CURVE('',#4298,#4303,#2583,.T.);
#5124=EDGE_CURVE('',#4304,#4304,#3856,.T.);
#5125=EDGE_CURVE('',#4304,#4305,#2584,.T.);
#5126=EDGE_CURVE('',#4305,#4305,#3857,.T.);
#5127=EDGE_CURVE('',#4306,#4306,#3858,.T.);
#5128=EDGE_CURVE('',#4306,#4307,#2585,.T.);
#5129=EDGE_CURVE('',#4307,#4307,#3859,.T.);
#5130=EDGE_CURVE('',#4308,#4309,#3860,.T.);
#5131=EDGE_CURVE('',#4310,#4311,#2586,.T.);
#5132=EDGE_CURVE('',#4310,#4312,#2587,.T.);
#5133=EDGE_CURVE('',#4311,#4312,#3861,.T.);
#5134=EDGE_CURVE('',#4313,#4314,#2588,.T.);
#5135=EDGE_CURVE('',#4315,#4313,#3862,.T.);
#5136=EDGE_CURVE('',#4315,#4314,#2589,.T.);
#5137=EDGE_CURVE('',#4316,#4317,#2590,.T.);
#5138=EDGE_CURVE('',#4318,#4316,#3863,.T.);
#5139=EDGE_CURVE('',#4318,#4317,#2591,.T.);
#5140=EDGE_CURVE('',#4317,#4310,#2592,.T.);
#5141=EDGE_CURVE('',#4312,#4318,#2593,.T.);
#5142=EDGE_CURVE('',#4319,#4320,#2594,.T.);
#5143=EDGE_CURVE('',#4319,#4321,#2595,.T.);
#5144=EDGE_CURVE('',#4320,#4321,#3864,.T.);
#5145=EDGE_CURVE('',#4314,#4319,#2596,.T.);
#5146=EDGE_CURVE('',#4321,#4315,#2597,.T.);
#5147=EDGE_CURVE('',#4322,#4323,#2598,.T.);
#5148=EDGE_CURVE('',#4323,#4324,#2599,.T.);
#5149=EDGE_CURVE('',#4324,#4325,#2600,.T.);
#5150=EDGE_CURVE('',#4325,#4322,#2601,.T.);
#5151=EDGE_CURVE('',#4326,#4326,#3865,.T.);
#5152=EDGE_CURVE('',#4327,#4327,#3866,.T.);
#5153=EDGE_CURVE('',#4320,#4328,#2602,.T.);
#5154=EDGE_CURVE('',#4328,#4329,#2603,.T.);
#5155=EDGE_CURVE('',#4329,#4316,#2604,.T.);
#5156=EDGE_CURVE('',#4311,#4330,#2605,.T.);
#5157=EDGE_CURVE('',#4330,#4331,#2606,.T.);
#5158=EDGE_CURVE('',#4331,#4313,#2607,.T.);
#5159=EDGE_CURVE('',#4330,#4331,#3867,.T.);
#5160=EDGE_CURVE('',#4328,#4329,#3868,.T.);
#5161=EDGE_CURVE('',#4332,#4333,#2608,.T.);
#5162=EDGE_CURVE('',#4332,#4334,#2609,.T.);
#5163=EDGE_CURVE('',#4334,#4335,#2610,.T.);
#5164=EDGE_CURVE('',#4333,#4335,#2611,.T.);
#5165=EDGE_CURVE('',#4336,#4332,#2612,.T.);
#5166=EDGE_CURVE('',#4336,#4337,#2613,.T.);
#5167=EDGE_CURVE('',#4337,#4334,#2614,.T.);
#5168=EDGE_CURVE('',#4338,#4336,#2615,.T.);
#5169=EDGE_CURVE('',#4338,#4339,#2616,.T.);
#5170=EDGE_CURVE('',#4339,#4337,#2617,.T.);
#5171=EDGE_CURVE('',#4333,#4338,#2618,.T.);
#5172=EDGE_CURVE('',#4335,#4339,#2619,.T.);
#5173=EDGE_CURVE('',#4340,#4340,#3869,.T.);
#5174=EDGE_CURVE('',#4340,#4327,#2620,.T.);
#5175=EDGE_CURVE('',#4341,#4341,#3870,.T.);
#5176=EDGE_CURVE('',#4341,#4326,#2621,.T.);
#5177=EDGE_CURVE('',#4342,#4343,#2622,.T.);
#5178=EDGE_CURVE('',#4343,#4322,#2623,.T.);
#5179=EDGE_CURVE('',#4342,#4325,#2624,.T.);
#5180=EDGE_CURVE('',#4344,#4342,#2625,.T.);
#5181=EDGE_CURVE('',#4344,#4324,#2626,.T.);
#5182=EDGE_CURVE('',#4345,#4344,#2627,.T.);
#5183=EDGE_CURVE('',#4345,#4323,#2628,.T.);
#5184=EDGE_CURVE('',#4343,#4345,#2629,.T.);
#5185=EDGE_CURVE('',#4346,#4346,#3871,.T.);
#5186=EDGE_CURVE('',#4346,#4347,#2630,.T.);
#5187=EDGE_CURVE('',#4347,#4347,#3872,.T.);
#5188=EDGE_CURVE('',#4348,#4348,#3873,.T.);
#5189=EDGE_CURVE('',#4349,#4350,#3874,.T.);
#5190=EDGE_CURVE('',#4351,#4351,#3875,.T.);
#5191=EDGE_CURVE('',#4352,#4353,#415,.T.);
#5192=EDGE_CURVE('',#4354,#4352,#416,.T.);
#5193=EDGE_CURVE('',#4353,#4354,#417,.T.);
#5194=EDGE_CURVE('',#4353,#4355,#2631,.T.);
#5195=EDGE_CURVE('',#4355,#4355,#418,.T.);
#5196=EDGE_CURVE('',#4356,#4356,#419,.T.);
#5197=EDGE_CURVE('',#4356,#4357,#2632,.T.);
#5198=EDGE_CURVE('',#4358,#4357,#420,.T.);
#5199=EDGE_CURVE('',#4359,#4358,#421,.T.);
#5200=EDGE_CURVE('',#4357,#4359,#422,.T.);
#5201=EDGE_CURVE('',#4360,#4360,#3876,.T.);
#5202=EDGE_CURVE('',#4360,#4361,#2633,.T.);
#5203=EDGE_CURVE('',#4361,#4361,#3877,.T.);
#5204=EDGE_CURVE('',#4362,#4363,#423,.T.);
#5205=EDGE_CURVE('',#4363,#4364,#424,.T.);
#5206=EDGE_CURVE('',#4364,#4362,#425,.T.);
#5207=EDGE_CURVE('',#4365,#4366,#426,.T.);
#5208=EDGE_CURVE('',#4366,#4367,#427,.T.);
#5209=EDGE_CURVE('',#4367,#4365,#428,.T.);
#5210=EDGE_CURVE('',#4368,#4369,#429,.T.);
#5211=EDGE_CURVE('',#4369,#4370,#430,.T.);
#5212=EDGE_CURVE('',#4370,#4368,#431,.T.);
#5213=EDGE_CURVE('',#4371,#4372,#432,.T.);
#5214=EDGE_CURVE('',#4372,#4373,#433,.T.);
#5215=EDGE_CURVE('',#4373,#4371,#434,.T.);
#5216=EDGE_CURVE('',#4364,#4374,#2634,.T.);
#5217=EDGE_CURVE('',#4374,#4374,#435,.T.);
#5218=EDGE_CURVE('',#4375,#4375,#436,.T.);
#5219=EDGE_CURVE('',#4375,#4367,#2635,.T.);
#5220=EDGE_CURVE('',#4370,#4376,#2636,.T.);
#5221=EDGE_CURVE('',#4376,#4376,#437,.T.);
#5222=EDGE_CURVE('',#4377,#4377,#438,.T.);
#5223=EDGE_CURVE('',#4377,#4373,#2637,.T.);
#5224=EDGE_CURVE('',#4378,#4378,#3878,.T.);
#5225=EDGE_CURVE('',#4379,#4379,#3879,.T.);
#5226=EDGE_CURVE('',#4380,#4380,#3880,.T.);
#5227=EDGE_CURVE('',#4380,#4379,#2638,.T.);
#5228=EDGE_CURVE('',#4381,#4381,#3881,.T.);
#5229=EDGE_CURVE('',#4381,#4378,#2639,.T.);
#5230=EDGE_CURVE('',#4382,#4382,#3882,.T.);
#5231=EDGE_CURVE('',#4382,#4383,#2640,.T.);
#5232=EDGE_CURVE('',#4383,#4383,#3883,.T.);
#5233=EDGE_CURVE('',#4384,#4384,#3884,.T.);
#5234=EDGE_CURVE('',#4384,#4385,#2641,.T.);
#5235=EDGE_CURVE('',#4385,#4385,#3885,.T.);
#5236=EDGE_CURVE('',#4386,#4387,#2642,.T.);
#5237=EDGE_CURVE('',#4387,#4388,#2643,.T.);
#5238=EDGE_CURVE('',#4388,#4389,#2644,.T.);
#5239=EDGE_CURVE('',#4386,#4389,#2645,.T.);
#5240=EDGE_CURVE('',#4387,#4390,#2646,.T.);
#5241=EDGE_CURVE('',#4390,#4391,#2647,.T.);
#5242=EDGE_CURVE('',#4391,#4388,#2648,.T.);
#5243=EDGE_CURVE('',#4390,#4392,#2649,.T.);
#5244=EDGE_CURVE('',#4392,#4393,#2650,.T.);
#5245=EDGE_CURVE('',#4393,#4391,#2651,.T.);
#5246=EDGE_CURVE('',#4392,#4394,#2652,.T.);
#5247=EDGE_CURVE('',#4394,#4395,#2653,.T.);
#5248=EDGE_CURVE('',#4395,#4393,#2654,.T.);
#5249=EDGE_CURVE('',#4394,#4396,#2655,.T.);
#5250=EDGE_CURVE('',#4396,#4397,#2656,.T.);
#5251=EDGE_CURVE('',#4397,#4395,#2657,.T.);
#5252=EDGE_CURVE('',#4396,#4386,#2658,.T.);
#5253=EDGE_CURVE('',#4389,#4397,#2659,.T.);
#5254=EDGE_CURVE('',#4398,#4398,#3886,.T.);
#5255=EDGE_CURVE('',#4399,#4399,#3887,.T.);
#5256=EDGE_CURVE('',#4400,#4400,#3888,.T.);
#5257=EDGE_CURVE('',#4400,#4399,#2660,.T.);
#5258=EDGE_CURVE('',#4401,#4401,#3889,.T.);
#5259=EDGE_CURVE('',#4401,#4400,#2661,.T.);
#5260=EDGE_CURVE('',#4402,#4402,#3890,.T.);
#5261=EDGE_CURVE('',#4402,#4401,#2662,.T.);
#5262=EDGE_CURVE('',#4403,#4403,#3891,.T.);
#5263=EDGE_CURVE('',#4404,#4404,#3892,.F.);
#5264=EDGE_CURVE('',#4404,#4403,#2663,.T.);
#5265=EDGE_CURVE('',#4398,#4404,#2664,.T.);
#5266=EDGE_CURVE('',#4405,#4405,#3893,.T.);
#5267=EDGE_CURVE('',#4405,#4406,#2665,.T.);
#5268=EDGE_CURVE('',#4406,#4406,#3894,.T.);
#5269=EDGE_CURVE('',#4407,#4407,#3895,.T.);
#5270=EDGE_CURVE('',#4408,#4408,#3896,.T.);
#5271=EDGE_CURVE('',#4408,#4409,#2666,.T.);
#5272=EDGE_CURVE('',#4409,#4409,#3897,.T.);
#5273=EDGE_CURVE('',#4410,#4410,#3898,.T.);
#5274=EDGE_CURVE('',#4411,#4411,#3899,.T.);
#5275=EDGE_CURVE('',#4411,#4412,#2667,.T.);
#5276=EDGE_CURVE('',#4412,#4412,#3900,.T.);
#5277=EDGE_CURVE('',#4413,#4413,#3901,.T.);
#5278=EDGE_CURVE('',#4414,#4414,#3902,.T.);
#5279=EDGE_CURVE('',#4414,#4415,#2668,.T.);
#5280=EDGE_CURVE('',#4415,#4415,#3903,.T.);
#5281=EDGE_CURVE('',#4416,#4416,#3904,.T.);
#5282=EDGE_CURVE('',#4417,#4417,#3905,.T.);
#5283=EDGE_CURVE('',#4417,#4407,#2669,.T.);
#5284=EDGE_CURVE('',#4418,#4418,#3906,.T.);
#5285=EDGE_CURVE('',#4418,#4410,#2670,.T.);
#5286=EDGE_CURVE('',#4419,#4419,#3907,.T.);
#5287=EDGE_CURVE('',#4419,#4413,#2671,.T.);
#5288=EDGE_CURVE('',#4420,#4420,#3908,.T.);
#5289=EDGE_CURVE('',#4420,#4416,#2672,.T.);
#5290=EDGE_CURVE('',#4421,#4422,#2673,.T.);
#5291=EDGE_CURVE('',#4422,#4423,#2674,.T.);
#5292=EDGE_CURVE('',#4424,#4423,#2675,.T.);
#5293=EDGE_CURVE('',#4421,#4424,#2676,.T.);
#5294=EDGE_CURVE('',#4425,#4421,#2677,.T.);
#5295=EDGE_CURVE('',#4426,#4424,#2678,.T.);
#5296=EDGE_CURVE('',#4425,#4426,#2679,.T.);
#5297=EDGE_CURVE('',#4427,#4425,#2680,.T.);
#5298=EDGE_CURVE('',#4428,#4426,#2681,.T.);
#5299=EDGE_CURVE('',#4427,#4428,#2682,.T.);
#5300=EDGE_CURVE('',#4429,#4427,#2683,.T.);
#5301=EDGE_CURVE('',#4430,#4428,#2684,.T.);
#5302=EDGE_CURVE('',#4429,#4430,#2685,.T.);
#5303=EDGE_CURVE('',#4431,#4429,#2686,.T.);
#5304=EDGE_CURVE('',#4432,#4430,#2687,.T.);
#5305=EDGE_CURVE('',#4431,#4432,#2688,.T.);
#5306=EDGE_CURVE('',#4433,#4431,#2689,.T.);
#5307=EDGE_CURVE('',#4434,#4432,#2690,.T.);
#5308=EDGE_CURVE('',#4433,#4434,#2691,.T.);
#5309=EDGE_CURVE('',#4435,#4433,#2692,.T.);
#5310=EDGE_CURVE('',#4436,#4434,#2693,.T.);
#5311=EDGE_CURVE('',#4435,#4436,#2694,.T.);
#5312=EDGE_CURVE('',#4437,#4435,#2695,.T.);
#5313=EDGE_CURVE('',#4438,#4436,#2696,.T.);
#5314=EDGE_CURVE('',#4437,#4438,#2697,.T.);
#5315=EDGE_CURVE('',#4439,#4437,#2698,.T.);
#5316=EDGE_CURVE('',#4440,#4438,#2699,.T.);
#5317=EDGE_CURVE('',#4439,#4440,#2700,.T.);
#5318=EDGE_CURVE('',#4441,#4439,#2701,.T.);
#5319=EDGE_CURVE('',#4442,#4440,#2702,.T.);
#5320=EDGE_CURVE('',#4441,#4442,#2703,.T.);
#5321=EDGE_CURVE('',#4443,#4441,#2704,.T.);
#5322=EDGE_CURVE('',#4444,#4442,#2705,.T.);
#5323=EDGE_CURVE('',#4443,#4444,#2706,.T.);
#5324=EDGE_CURVE('',#4422,#4443,#2707,.T.);
#5325=EDGE_CURVE('',#4423,#4444,#2708,.T.);
#5326=EDGE_CURVE('',#4445,#4445,#3909,.T.);
#5327=EDGE_CURVE('',#4446,#4446,#3910,.T.);
#5328=EDGE_CURVE('',#4446,#4445,#2709,.T.);
#5329=EDGE_CURVE('',#4447,#4447,#3911,.T.);
#5330=EDGE_CURVE('',#4447,#4446,#2710,.T.);
#5331=EDGE_CURVE('',#4448,#4448,#3912,.T.);
#5332=EDGE_CURVE('',#4448,#4447,#2711,.T.);
#5333=EDGE_CURVE('',#4449,#4449,#3913,.T.);
#5334=EDGE_CURVE('',#4450,#4450,#3914,.F.);
#5335=EDGE_CURVE('',#4450,#4449,#2712,.T.);
#5336=EDGE_CURVE('',#4451,#4451,#3915,.F.);
#5337=EDGE_CURVE('',#4451,#4450,#2713,.T.);
#5338=EDGE_CURVE('',#4452,#4452,#3916,.T.);
#5339=EDGE_CURVE('',#4452,#4451,#2714,.T.);
#5340=EDGE_CURVE('',#4453,#4454,#2715,.T.);
#5341=EDGE_CURVE('',#4454,#4455,#2716,.T.);
#5342=EDGE_CURVE('',#4455,#4456,#2717,.T.);
#5343=EDGE_CURVE('',#4453,#4456,#2718,.T.);
#5344=EDGE_CURVE('',#4454,#4457,#2719,.T.);
#5345=EDGE_CURVE('',#4457,#4458,#2720,.T.);
#5346=EDGE_CURVE('',#4458,#4455,#2721,.T.);
#5347=EDGE_CURVE('',#4457,#4459,#2722,.T.);
#5348=EDGE_CURVE('',#4459,#4460,#2723,.T.);
#5349=EDGE_CURVE('',#4460,#4458,#2724,.T.);
#5350=EDGE_CURVE('',#4459,#4461,#2725,.T.);
#5351=EDGE_CURVE('',#4461,#4462,#2726,.T.);
#5352=EDGE_CURVE('',#4462,#4460,#2727,.T.);
#5353=EDGE_CURVE('',#4461,#4463,#2728,.T.);
#5354=EDGE_CURVE('',#4463,#4464,#2729,.T.);
#5355=EDGE_CURVE('',#4464,#4462,#2730,.T.);
#5356=EDGE_CURVE('',#4463,#4453,#2731,.T.);
#5357=EDGE_CURVE('',#4456,#4464,#2732,.T.);
#5358=EDGE_CURVE('',#4465,#4466,#2733,.T.);
#5359=EDGE_CURVE('',#4467,#4465,#2734,.T.);
#5360=EDGE_CURVE('',#4468,#4467,#2735,.T.);
#5361=EDGE_CURVE('',#4468,#4466,#2736,.T.);
#5362=EDGE_CURVE('',#4466,#4469,#3917,.T.);
#5363=EDGE_CURVE('',#4470,#4468,#2737,.T.);
#5364=EDGE_CURVE('',#4469,#4470,#2738,.T.);
#5365=EDGE_CURVE('',#4469,#4471,#2739,.T.);
#5366=EDGE_CURVE('',#4470,#4472,#2740,.T.);
#5367=EDGE_CURVE('',#4471,#4472,#2741,.T.);
#5368=EDGE_CURVE('',#4472,#4467,#2742,.T.);
#5369=EDGE_CURVE('',#4473,#4471,#3918,.T.);
#5370=EDGE_CURVE('',#4473,#4474,#2743,.T.);
#5371=EDGE_CURVE('',#4474,#4474,#3919,.T.);
#5372=EDGE_CURVE('',#4465,#4473,#3920,.T.);
#5373=EDGE_CURVE('',#4475,#4476,#2744,.T.);
#5374=EDGE_CURVE('',#4475,#4476,#3921,.T.);
#5375=EDGE_CURVE('',#4477,#4475,#439,.T.);
#5376=EDGE_CURVE('',#4478,#4477,#3922,.T.);
#5377=EDGE_CURVE('',#4478,#4479,#2745,.T.);
#5378=EDGE_CURVE('',#4480,#4479,#440,.T.);
#5379=EDGE_CURVE('',#4479,#4480,#441,.T.);
#5380=EDGE_CURVE('',#4481,#4478,#3923,.T.);
#5381=EDGE_CURVE('',#4476,#4481,#442,.T.);
#5382=EDGE_CURVE('',#4481,#4477,#2746,.T.);
#5383=EDGE_CURVE('',#4482,#4482,#3924,.T.);
#5384=EDGE_CURVE('',#4482,#4483,#2747,.T.);
#5385=EDGE_CURVE('',#4483,#4483,#3925,.T.);
#5386=EDGE_CURVE('',#4484,#4484,#3926,.T.);
#5387=EDGE_CURVE('',#4484,#4485,#2748,.T.);
#5388=EDGE_CURVE('',#4485,#4485,#3927,.T.);
#5389=EDGE_CURVE('',#4486,#4487,#2749,.T.);
#5390=EDGE_CURVE('',#4486,#4487,#3928,.T.);
#5391=EDGE_CURVE('',#4488,#4486,#443,.T.);
#5392=EDGE_CURVE('',#4489,#4488,#3929,.T.);
#5393=EDGE_CURVE('',#4489,#4490,#2750,.T.);
#5394=EDGE_CURVE('',#4491,#4490,#444,.T.);
#5395=EDGE_CURVE('',#4490,#4491,#445,.T.);
#5396=EDGE_CURVE('',#4492,#4489,#3930,.T.);
#5397=EDGE_CURVE('',#4487,#4492,#446,.T.);
#5398=EDGE_CURVE('',#4492,#4488,#2751,.T.);
#5399=EDGE_CURVE('',#4493,#4493,#3931,.T.);
#5400=EDGE_CURVE('',#4493,#4494,#2752,.T.);
#5401=EDGE_CURVE('',#4494,#4494,#3932,.T.);
#5402=EDGE_CURVE('',#4495,#4495,#3933,.T.);
#5403=EDGE_CURVE('',#4495,#4496,#2753,.T.);
#5404=EDGE_CURVE('',#4496,#4496,#3934,.T.);
#5405=EDGE_CURVE('',#4497,#4497,#3935,.T.);
#5406=EDGE_CURVE('',#4497,#4498,#2754,.T.);
#5407=EDGE_CURVE('',#4498,#4498,#3936,.T.);
#5408=EDGE_CURVE('',#4499,#4499,#3937,.T.);
#5409=EDGE_CURVE('',#4499,#4500,#2755,.T.);
#5410=EDGE_CURVE('',#4500,#4500,#3938,.T.);
#5411=EDGE_CURVE('',#4501,#4502,#3939,.T.);
#5412=EDGE_CURVE('',#4501,#4502,#3940,.T.);
#5413=EDGE_CURVE('',#4503,#4501,#2756,.T.);
#5414=EDGE_CURVE('',#4504,#4503,#3941,.T.);
#5415=EDGE_CURVE('',#4504,#4505,#2757,.T.);
#5416=EDGE_CURVE('',#4505,#4505,#3942,.T.);
#5417=EDGE_CURVE('',#4506,#4504,#3943,.T.);
#5418=EDGE_CURVE('',#4502,#4506,#2758,.T.);
#5419=EDGE_CURVE('',#4506,#4507,#3944,.T.);
#5420=EDGE_CURVE('',#4507,#4508,#2759,.T.);
#5421=EDGE_CURVE('',#4508,#4509,#3945,.T.);
#5422=EDGE_CURVE('',#4509,#4510,#447,.T.);
#5423=EDGE_CURVE('',#4510,#4511,#2760,.T.);
#5424=EDGE_CURVE('',#4511,#4512,#448,.T.);
#5425=EDGE_CURVE('',#4512,#4513,#2761,.T.);
#5426=EDGE_CURVE('',#4513,#4514,#449,.T.);
#5427=EDGE_CURVE('',#4514,#4515,#3946,.T.);
#5428=EDGE_CURVE('',#4515,#4516,#2762,.T.);
#5429=EDGE_CURVE('',#4516,#4503,#3947,.T.);
#5430=EDGE_CURVE('',#4517,#4516,#2763,.T.);
#5431=EDGE_CURVE('',#4518,#4517,#2764,.T.);
#5432=EDGE_CURVE('',#4507,#4518,#2765,.T.);
#5433=EDGE_CURVE('',#4519,#4519,#3948,.T.);
#5434=EDGE_CURVE('',#4520,#4517,#2766,.T.);
#5435=EDGE_CURVE('',#4521,#4520,#2767,.T.);
#5436=EDGE_CURVE('',#4521,#4518,#2768,.T.);
#5437=EDGE_CURVE('',#4520,#4515,#2769,.T.);
#5438=EDGE_CURVE('',#4512,#4513,#3949,.T.);
#5439=EDGE_CURVE('',#4510,#4511,#3950,.T.);
#5440=EDGE_CURVE('',#4522,#4509,#2770,.T.);
#5441=EDGE_CURVE('',#4523,#4522,#450,.T.);
#5442=EDGE_CURVE('',#4514,#4523,#2771,.T.);
#5443=EDGE_CURVE('',#4508,#4521,#2772,.T.);
#5444=EDGE_CURVE('',#4524,#4524,#3951,.T.);
#5445=EDGE_CURVE('',#4525,#4525,#3952,.T.);
#5446=EDGE_CURVE('',#4519,#4524,#2773,.T.);
#5447=EDGE_CURVE('',#4525,#4526,#2774,.T.);
#5448=EDGE_CURVE('',#4526,#4523,#3953,.T.);
#5449=EDGE_CURVE('',#4522,#4526,#3954,.T.);
#5450=EDGE_CURVE('',#4527,#4527,#3955,.T.);
#5451=EDGE_CURVE('',#4527,#4528,#2775,.T.);
#5452=EDGE_CURVE('',#4528,#4528,#3956,.T.);
#5453=EDGE_CURVE('',#4529,#4529,#3957,.T.);
#5454=EDGE_CURVE('',#4530,#4530,#3958,.T.);
#5455=EDGE_CURVE('',#4531,#4531,#3959,.T.);
#5456=EDGE_CURVE('',#4531,#4529,#2776,.T.);
#5457=EDGE_CURVE('',#4530,#4532,#2777,.T.);
#5458=EDGE_CURVE('',#4532,#4532,#3960,.T.);
#5459=EDGE_CURVE('',#4533,#4533,#3961,.T.);
#5460=EDGE_CURVE('',#4533,#4534,#2778,.T.);
#5461=EDGE_CURVE('',#4534,#4534,#3962,.T.);
#5462=EDGE_CURVE('',#4535,#4535,#3963,.T.);
#5463=EDGE_CURVE('',#4535,#4536,#2779,.T.);
#5464=EDGE_CURVE('',#4536,#4536,#3964,.T.);
#5465=EDGE_CURVE('',#4537,#4537,#3965,.T.);
#5466=EDGE_CURVE('',#4537,#4538,#2780,.T.);
#5467=EDGE_CURVE('',#4538,#4538,#3966,.T.);
#5468=EDGE_CURVE('',#4539,#4539,#3967,.T.);
#5469=EDGE_CURVE('',#4539,#4540,#2781,.T.);
#5470=EDGE_CURVE('',#4540,#4540,#3968,.T.);
#5471=EDGE_CURVE('',#4541,#4541,#3969,.T.);
#5472=EDGE_CURVE('',#4541,#4542,#2782,.T.);
#5473=EDGE_CURVE('',#4542,#4542,#3970,.T.);
#5474=EDGE_CURVE('',#4543,#4543,#3971,.T.);
#5475=EDGE_CURVE('',#4543,#4544,#2783,.T.);
#5476=EDGE_CURVE('',#4544,#4544,#3972,.T.);
#5477=EDGE_CURVE('',#4545,#4546,#2784,.T.);
#5478=EDGE_CURVE('',#4547,#4545,#2785,.T.);
#5479=EDGE_CURVE('',#4548,#4547,#2786,.T.);
#5480=EDGE_CURVE('',#4549,#4548,#2787,.T.);
#5481=EDGE_CURVE('',#4550,#4549,#2788,.T.);
#5482=EDGE_CURVE('',#4551,#4550,#2789,.T.);
#5483=EDGE_CURVE('',#4552,#4551,#2790,.T.);
#5484=EDGE_CURVE('',#4546,#4552,#2791,.T.);
#5485=EDGE_CURVE('',#4549,#4553,#2792,.T.);
#5486=EDGE_CURVE('',#4553,#4554,#2793,.T.);
#5487=EDGE_CURVE('',#4554,#4550,#2794,.T.);
#5488=EDGE_CURVE('',#4555,#4548,#2795,.T.);
#5489=EDGE_CURVE('',#4555,#4553,#2796,.T.);
#5490=EDGE_CURVE('',#4547,#4556,#2797,.T.);
#5491=EDGE_CURVE('',#4556,#4555,#2798,.T.);
#5492=EDGE_CURVE('',#4557,#4545,#2799,.T.);
#5493=EDGE_CURVE('',#4557,#4556,#2800,.T.);
#5494=EDGE_CURVE('',#4558,#4559,#2801,.T.);
#5495=EDGE_CURVE('',#4554,#4558,#2802,.T.);
#5496=EDGE_CURVE('',#4560,#4557,#2803,.T.);
#5497=EDGE_CURVE('',#4559,#4560,#2804,.T.);
#5498=EDGE_CURVE('',#4551,#4558,#2805,.T.);
#5499=EDGE_CURVE('',#4546,#4560,#2806,.T.);
#5500=EDGE_CURVE('',#4559,#4552,#2807,.T.);
#5501=EDGE_CURVE('',#4561,#4562,#2808,.T.);
#5502=EDGE_CURVE('',#4561,#4563,#2809,.T.);
#5503=EDGE_CURVE('',#4563,#4564,#2810,.T.);
#5504=EDGE_CURVE('',#4562,#4564,#2811,.T.);
#5505=EDGE_CURVE('',#4565,#4561,#2812,.T.);
#5506=EDGE_CURVE('',#4565,#4566,#2813,.T.);
#5507=EDGE_CURVE('',#4566,#4563,#2814,.T.);
#5508=EDGE_CURVE('',#4567,#4565,#2815,.T.);
#5509=EDGE_CURVE('',#4567,#4568,#2816,.T.);
#5510=EDGE_CURVE('',#4568,#4566,#2817,.T.);
#5511=EDGE_CURVE('',#4569,#4567,#2818,.T.);
#5512=EDGE_CURVE('',#4569,#4570,#2819,.T.);
#5513=EDGE_CURVE('',#4570,#4568,#2820,.T.);
#5514=EDGE_CURVE('',#4571,#4569,#2821,.T.);
#5515=EDGE_CURVE('',#4571,#4572,#2822,.T.);
#5516=EDGE_CURVE('',#4572,#4570,#2823,.T.);
#5517=EDGE_CURVE('',#4562,#4571,#2824,.T.);
#5518=EDGE_CURVE('',#4564,#4572,#2825,.T.);
#5519=EDGE_CURVE('',#4573,#4573,#3973,.T.);
#5520=EDGE_CURVE('',#4574,#4574,#3974,.T.);
#5521=EDGE_CURVE('',#4574,#4573,#2826,.T.);
#5522=EDGE_CURVE('',#4575,#4575,#3975,.F.);
#5523=EDGE_CURVE('',#4575,#4574,#2827,.T.);
#5524=EDGE_CURVE('',#4576,#4576,#3976,.T.);
#5525=EDGE_CURVE('',#4576,#4575,#2828,.T.);
#5526=EDGE_CURVE('',#4577,#4577,#3977,.T.);
#5527=EDGE_CURVE('',#4577,#4578,#2829,.T.);
#5528=EDGE_CURVE('',#4578,#4578,#3978,.T.);
#5529=EDGE_CURVE('',#4579,#4579,#3979,.T.);
#5530=EDGE_CURVE('',#4579,#4580,#2830,.T.);
#5531=EDGE_CURVE('',#4580,#4580,#3980,.T.);
#5532=EDGE_CURVE('',#4581,#4582,#2831,.T.);
#5533=EDGE_CURVE('',#4581,#4583,#3981,.T.);
#5534=EDGE_CURVE('',#4584,#4583,#2832,.T.);
#5535=EDGE_CURVE('',#4582,#4584,#3982,.T.);
#5536=EDGE_CURVE('',#4584,#4585,#2833,.T.);
#5537=EDGE_CURVE('',#4585,#4586,#3983,.T.);
#5538=EDGE_CURVE('',#4586,#4582,#2834,.T.);
#5539=EDGE_CURVE('',#4587,#4583,#2835,.T.);
#5540=EDGE_CURVE('',#4587,#4585,#2836,.T.);
#5541=EDGE_CURVE('',#4586,#4588,#2837,.T.);
#5542=EDGE_CURVE('',#4587,#4588,#3984,.T.);
#5543=EDGE_CURVE('',#4581,#4588,#2838,.T.);
#5544=EDGE_CURVE('',#4589,#4589,#3985,.T.);
#5545=EDGE_CURVE('',#4589,#4590,#2839,.T.);
#5546=EDGE_CURVE('',#4590,#4590,#3986,.T.);
#5547=EDGE_CURVE('',#4591,#4591,#3987,.T.);
#5548=EDGE_CURVE('',#4591,#4592,#2840,.T.);
#5549=EDGE_CURVE('',#4592,#4592,#3988,.T.);
#5550=EDGE_CURVE('',#4593,#4593,#3989,.T.);
#5551=EDGE_CURVE('',#4593,#4594,#2841,.T.);
#5552=EDGE_CURVE('',#4594,#4594,#3990,.T.);
#5553=EDGE_CURVE('',#4595,#4595,#3991,.T.);
#5554=EDGE_CURVE('',#4595,#4596,#2842,.T.);
#5555=EDGE_CURVE('',#4596,#4596,#3992,.T.);
#5556=EDGE_CURVE('',#4597,#4597,#3993,.T.);
#5557=EDGE_CURVE('',#4597,#4598,#2843,.T.);
#5558=EDGE_CURVE('',#4598,#4598,#3994,.T.);
#5559=EDGE_CURVE('',#4599,#4599,#3995,.T.);
#5560=EDGE_CURVE('',#4599,#4600,#2844,.T.);
#5561=EDGE_CURVE('',#4600,#4600,#3996,.T.);
#5562=EDGE_CURVE('',#4601,#4601,#3997,.T.);
#5563=EDGE_CURVE('',#4601,#4602,#2845,.T.);
#5564=EDGE_CURVE('',#4602,#4602,#3998,.T.);
#5565=EDGE_CURVE('',#4603,#4603,#3999,.T.);
#5566=EDGE_CURVE('',#4603,#4604,#2846,.T.);
#5567=EDGE_CURVE('',#4604,#4604,#4000,.T.);
#5568=EDGE_CURVE('',#4605,#4606,#4001,.T.);
#5569=EDGE_CURVE('',#4606,#4605,#4002,.T.);
#5570=EDGE_CURVE('',#4606,#4607,#4003,.T.);
#5571=EDGE_CURVE('',#4608,#4607,#4004,.T.);
#5572=EDGE_CURVE('',#4607,#4608,#4005,.T.);
#5573=EDGE_CURVE('',#4608,#4609,#2847,.T.);
#5574=EDGE_CURVE('',#4609,#4609,#4006,.T.);
#5575=EDGE_CURVE('',#4610,#4610,#4007,.T.);
#5576=EDGE_CURVE('',#4610,#4611,#2848,.T.);
#5577=EDGE_CURVE('',#4611,#4611,#4008,.T.);
#5578=EDGE_CURVE('',#4611,#4612,#2849,.T.);
#5579=EDGE_CURVE('',#4612,#4612,#4009,.T.);
#5580=EDGE_CURVE('',#4613,#4613,#4010,.T.);
#5581=EDGE_CURVE('',#4613,#4605,#2850,.T.);
#5582=EDGE_CURVE('',#4614,#4614,#4011,.T.);
#5583=EDGE_CURVE('',#4614,#4610,#2851,.T.);
#5584=EDGE_CURVE('',#4615,#4616,#4012,.T.);
#5585=EDGE_CURVE('',#4616,#4615,#4013,.T.);
#5586=EDGE_CURVE('',#4616,#4617,#4014,.T.);
#5587=EDGE_CURVE('',#4618,#4617,#4015,.T.);
#5588=EDGE_CURVE('',#4617,#4618,#4016,.T.);
#5589=EDGE_CURVE('',#4619,#4619,#4017,.T.);
#5590=EDGE_CURVE('',#4619,#4618,#2852,.T.);
#5591=EDGE_CURVE('',#4620,#4620,#4018,.T.);
#5592=EDGE_CURVE('',#4621,#4621,#4019,.T.);
#5593=EDGE_CURVE('',#4622,#4622,#4020,.T.);
#5594=EDGE_CURVE('',#4622,#4620,#2853,.T.);
#5595=EDGE_CURVE('',#4623,#4623,#4021,.T.);
#5596=EDGE_CURVE('',#4623,#4622,#2854,.T.);
#5597=EDGE_CURVE('',#4624,#4624,#4022,.T.);
#5598=EDGE_CURVE('',#4624,#4623,#2855,.T.);
#5599=EDGE_CURVE('',#4615,#4621,#2856,.T.);
#5600=EDGE_CURVE('',#4625,#4626,#4023,.T.);
#5601=EDGE_CURVE('',#4627,#4628,#4024,.T.);
#5602=EDGE_CURVE('',#4629,#4630,#4025,.T.);
#5603=EDGE_CURVE('',#4631,#4632,#4026,.T.);
#5604=EDGE_CURVE('',#4633,#4634,#4027,.T.);
#5605=EDGE_CURVE('',#4635,#4636,#4028,.T.);
#5606=EDGE_CURVE('',#4637,#4638,#4029,.T.);
#5607=EDGE_CURVE('',#4639,#4640,#4030,.T.);
#5608=EDGE_CURVE('',#4641,#4642,#451,.T.);
#5609=EDGE_CURVE('',#4643,#4641,#4031,.T.);
#5610=EDGE_CURVE('',#4644,#4643,#452,.T.);
#5611=EDGE_CURVE('',#4642,#4644,#4032,.T.);
#5612=EDGE_CURVE('',#4645,#4643,#4033,.T.);
#5613=EDGE_CURVE('',#4645,#4646,#453,.T.);
#5614=EDGE_CURVE('',#4647,#4646,#4034,.T.);
#5615=EDGE_CURVE('',#4647,#4648,#454,.T.);
#5616=EDGE_CURVE('',#4649,#4648,#4035,.T.);
#5617=EDGE_CURVE('',#4649,#4650,#455,.T.);
#5618=EDGE_CURVE('',#4650,#4651,#2857,.T.);
#5619=EDGE_CURVE('',#4651,#4651,#4036,.T.);
#5620=EDGE_CURVE('',#4650,#4652,#456,.T.);
#5621=EDGE_CURVE('',#4653,#4652,#4037,.T.);
#5622=EDGE_CURVE('',#4653,#4654,#457,.T.);
#5623=EDGE_CURVE('',#4655,#4654,#4038,.T.);
#5624=EDGE_CURVE('',#4655,#4656,#458,.T.);
#5625=EDGE_CURVE('',#4657,#4656,#4039,.T.);
#5626=EDGE_CURVE('',#4657,#4658,#459,.T.);
#5627=EDGE_CURVE('',#4659,#4658,#4040,.T.);
#5628=EDGE_CURVE('',#4659,#4660,#460,.T.);
#5629=EDGE_CURVE('',#4644,#4660,#4041,.T.);
#5630=EDGE_CURVE('',#4641,#4661,#4042,.T.);
#5631=EDGE_CURVE('',#4661,#4645,#4043,.T.);
#5632=EDGE_CURVE('',#4662,#4661,#461,.T.);
#5633=EDGE_CURVE('',#4646,#4662,#4044,.T.);
#5634=EDGE_CURVE('',#4662,#4663,#4045,.T.);
#5635=EDGE_CURVE('',#4663,#4647,#4046,.T.);
#5636=EDGE_CURVE('',#4664,#4663,#462,.T.);
#5637=EDGE_CURVE('',#4648,#4664,#4047,.T.);
#5638=EDGE_CURVE('',#4664,#4665,#4048,.T.);
#5639=EDGE_CURVE('',#4665,#4649,#4049,.T.);
#5640=EDGE_CURVE('',#4666,#4667,#463,.T.);
#5641=EDGE_CURVE('',#4652,#4666,#4050,.T.);
#5642=EDGE_CURVE('',#4667,#4665,#464,.T.);
#5643=EDGE_CURVE('',#4666,#4668,#4051,.T.);
#5644=EDGE_CURVE('',#4668,#4653,#4052,.T.);
#5645=EDGE_CURVE('',#4669,#4668,#465,.T.);
#5646=EDGE_CURVE('',#4654,#4669,#4053,.T.);
#5647=EDGE_CURVE('',#4669,#4670,#4054,.T.);
#5648=EDGE_CURVE('',#4670,#4655,#4055,.T.);
#5649=EDGE_CURVE('',#4671,#4670,#466,.T.);
#5650=EDGE_CURVE('',#4656,#4671,#4056,.T.);
#5651=EDGE_CURVE('',#4671,#4672,#4057,.T.);
#5652=EDGE_CURVE('',#4672,#4657,#4058,.T.);
#5653=EDGE_CURVE('',#4673,#4672,#467,.T.);
#5654=EDGE_CURVE('',#4658,#4673,#4059,.T.);
#5655=EDGE_CURVE('',#4674,#4674,#4060,.T.);
#5656=EDGE_CURVE('',#4674,#4667,#2858,.T.);
#5657=EDGE_CURVE('',#4675,#4642,#4061,.T.);
#5658=EDGE_CURVE('',#4675,#4676,#468,.T.);
#5659=EDGE_CURVE('',#4673,#4676,#4062,.T.);
#5660=EDGE_CURVE('',#4660,#4675,#4063,.T.);
#5661=EDGE_CURVE('',#4676,#4659,#4064,.T.);
#5662=EDGE_CURVE('',#4677,#4677,#4065,.T.);
#5663=EDGE_CURVE('',#4678,#4678,#4066,.T.);
#5664=EDGE_CURVE('',#4679,#4679,#4067,.T.);
#5665=EDGE_CURVE('',#4679,#4677,#2859,.T.);
#5666=EDGE_CURVE('',#4680,#4680,#4068,.T.);
#5667=EDGE_CURVE('',#4680,#4678,#2860,.T.);
#5668=EDGE_CURVE('',#4681,#4681,#4069,.T.);
#5669=EDGE_CURVE('',#4682,#4682,#4070,.T.);
#5670=EDGE_CURVE('',#4683,#4683,#4071,.T.);
#5671=EDGE_CURVE('',#4683,#4681,#2861,.T.);
#5672=EDGE_CURVE('',#4684,#4684,#4072,.T.);
#5673=EDGE_CURVE('',#4684,#4682,#2862,.T.);
#5674=EDGE_CURVE('',#4685,#4685,#4073,.T.);
#5675=EDGE_CURVE('',#4685,#4686,#2863,.T.);
#5676=EDGE_CURVE('',#4686,#4686,#4074,.T.);
#5677=EDGE_CURVE('',#4687,#4687,#4075,.T.);
#5678=EDGE_CURVE('',#4687,#4688,#2864,.T.);
#5679=EDGE_CURVE('',#4688,#4688,#4076,.T.);
#5680=EDGE_CURVE('',#4689,#4690,#2865,.T.);
#5681=EDGE_CURVE('',#4689,#4691,#2866,.T.);
#5682=EDGE_CURVE('',#4692,#4691,#2867,.T.);
#5683=EDGE_CURVE('',#4690,#4692,#2868,.T.);
#5684=EDGE_CURVE('',#4693,#4694,#2869,.T.);
#5685=EDGE_CURVE('',#4695,#4693,#2870,.T.);
#5686=EDGE_CURVE('',#4696,#4695,#2871,.T.);
#5687=EDGE_CURVE('',#4694,#4696,#2872,.T.);
#5688=EDGE_CURVE('',#4694,#4689,#2873,.T.);
#5689=EDGE_CURVE('',#4691,#4696,#2874,.T.);
#5690=EDGE_CURVE('',#4692,#4695,#2875,.T.);
#5691=EDGE_CURVE('',#4697,#4697,#4077,.T.);
#5692=EDGE_CURVE('',#4697,#4698,#2876,.T.);
#5693=EDGE_CURVE('',#4698,#4698,#4078,.T.);
#5694=EDGE_CURVE('',#4699,#4700,#2877,.T.);
#5695=EDGE_CURVE('',#4699,#4701,#2878,.T.);
#5696=EDGE_CURVE('',#4701,#4702,#2879,.T.);
#5697=EDGE_CURVE('',#4702,#4700,#2880,.T.);
#5698=EDGE_CURVE('',#4703,#4699,#2881,.T.);
#5699=EDGE_CURVE('',#4704,#4703,#2882,.T.);
#5700=EDGE_CURVE('',#4701,#4704,#2883,.T.);
#5701=EDGE_CURVE('',#4700,#4705,#2884,.T.);
#5702=EDGE_CURVE('',#4702,#4706,#2885,.T.);
#5703=EDGE_CURVE('',#4705,#4706,#2886,.T.);
#5704=EDGE_CURVE('',#4706,#4704,#2887,.T.);
#5705=EDGE_CURVE('',#4705,#4703,#2888,.T.);
#5706=EDGE_CURVE('',#4707,#4707,#4079,.T.);
#5707=EDGE_CURVE('',#4707,#4708,#2889,.T.);
#5708=EDGE_CURVE('',#4708,#4708,#4080,.T.);
#5709=EDGE_CURVE('',#4709,#4709,#4081,.T.);
#5710=EDGE_CURVE('',#4709,#4710,#2890,.T.);
#5711=EDGE_CURVE('',#4710,#4710,#4082,.T.);
#5712=EDGE_CURVE('',#4711,#4711,#4083,.T.);
#5713=EDGE_CURVE('',#4711,#4712,#2891,.T.);
#5714=EDGE_CURVE('',#4712,#4712,#4084,.T.);
#5715=EDGE_CURVE('',#4713,#4713,#4085,.T.);
#5716=EDGE_CURVE('',#4713,#4714,#2892,.T.);
#5717=EDGE_CURVE('',#4714,#4714,#4086,.T.);
#5718=EDGE_CURVE('',#4715,#4716,#2893,.T.);
#5719=EDGE_CURVE('',#4716,#4717,#2894,.T.);
#5720=EDGE_CURVE('',#4718,#4717,#2895,.T.);
#5721=EDGE_CURVE('',#4715,#4718,#2896,.T.);
#5722=EDGE_CURVE('',#4719,#4715,#2897,.T.);
#5723=EDGE_CURVE('',#4720,#4718,#2898,.T.);
#5724=EDGE_CURVE('',#4719,#4720,#2899,.T.);
#5725=EDGE_CURVE('',#4721,#4719,#2900,.T.);
#5726=EDGE_CURVE('',#4693,#4720,#2901,.T.);
#5727=EDGE_CURVE('',#4722,#4690,#2902,.T.);
#5728=EDGE_CURVE('',#4721,#4722,#2903,.T.);
#5729=EDGE_CURVE('',#4716,#4721,#2904,.T.);
#5730=EDGE_CURVE('',#4717,#4722,#2905,.T.);
#5731=EDGE_CURVE('',#4723,#4723,#4087,.T.);
#5732=EDGE_CURVE('',#4723,#4724,#2906,.T.);
#5733=EDGE_CURVE('',#4724,#4724,#4088,.T.);
#5734=EDGE_CURVE('',#4725,#4725,#4089,.T.);
#5735=EDGE_CURVE('',#4725,#4726,#2907,.T.);
#5736=EDGE_CURVE('',#4726,#4726,#4090,.T.);
#5737=EDGE_CURVE('',#4727,#4728,#2908,.T.);
#5738=EDGE_CURVE('',#4728,#4729,#2909,.T.);
#5739=EDGE_CURVE('',#4730,#4729,#2910,.T.);
#5740=EDGE_CURVE('',#4727,#4730,#2911,.T.);
#5741=EDGE_CURVE('',#4731,#4727,#2912,.T.);
#5742=EDGE_CURVE('',#4732,#4730,#2913,.T.);
#5743=EDGE_CURVE('',#4731,#4732,#2914,.T.);
#5744=EDGE_CURVE('',#4733,#4731,#2915,.T.);
#5745=EDGE_CURVE('',#4734,#4732,#2916,.T.);
#5746=EDGE_CURVE('',#4733,#4734,#2917,.T.);
#5747=EDGE_CURVE('',#4728,#4733,#2918,.T.);
#5748=EDGE_CURVE('',#4729,#4734,#2919,.T.);
#5749=EDGE_CURVE('',#4735,#4735,#4091,.T.);
#5750=EDGE_CURVE('',#4735,#4736,#2920,.T.);
#5751=EDGE_CURVE('',#4736,#4736,#4092,.T.);
#5752=EDGE_CURVE('',#4737,#4737,#4093,.T.);
#5753=EDGE_CURVE('',#4738,#4738,#4094,.T.);
#5754=EDGE_CURVE('',#4737,#4739,#2921,.T.);
#5755=EDGE_CURVE('',#4739,#4739,#4095,.T.);
#5756=EDGE_CURVE('',#4740,#4740,#4096,.T.);
#5757=EDGE_CURVE('',#4740,#4738,#2922,.T.);
#5758=EDGE_CURVE('',#4741,#4741,#4097,.T.);
#5759=EDGE_CURVE('',#4741,#4742,#2923,.T.);
#5760=EDGE_CURVE('',#4742,#4742,#4098,.T.);
#5761=EDGE_CURVE('',#4743,#4743,#4099,.T.);
#5762=EDGE_CURVE('',#4743,#4744,#2924,.T.);
#5763=EDGE_CURVE('',#4744,#4744,#4100,.T.);
#5764=EDGE_CURVE('',#4745,#4745,#4101,.T.);
#5765=EDGE_CURVE('',#4745,#4746,#2925,.T.);
#5766=EDGE_CURVE('',#4746,#4746,#4102,.T.);
#5767=EDGE_CURVE('',#4747,#4747,#4103,.T.);
#5768=EDGE_CURVE('',#4747,#4748,#2926,.T.);
#5769=EDGE_CURVE('',#4748,#4748,#4104,.T.);
#5770=EDGE_CURVE('',#4749,#4749,#4105,.T.);
#5771=EDGE_CURVE('',#4749,#4750,#2927,.T.);
#5772=EDGE_CURVE('',#4750,#4750,#4106,.T.);
#5773=EDGE_CURVE('',#4751,#4751,#4107,.T.);
#5774=EDGE_CURVE('',#4751,#4752,#2928,.T.);
#5775=EDGE_CURVE('',#4752,#4752,#4108,.T.);
#5776=EDGE_CURVE('',#4753,#4754,#2929,.T.);
#5777=EDGE_CURVE('',#4753,#4754,#4109,.T.);
#5778=EDGE_CURVE('',#4755,#4753,#2930,.T.);
#5779=EDGE_CURVE('',#4756,#4755,#4110,.T.);
#5780=EDGE_CURVE('',#4756,#4757,#2931,.T.);
#5781=EDGE_CURVE('',#4757,#4757,#4111,.T.);
#5782=EDGE_CURVE('',#4758,#4756,#4112,.T.);
#5783=EDGE_CURVE('',#4754,#4758,#2932,.T.);
#5784=EDGE_CURVE('',#4759,#4760,#2933,.T.);
#5785=EDGE_CURVE('',#4759,#4760,#4113,.T.);
#5786=EDGE_CURVE('',#4761,#4759,#2934,.T.);
#5787=EDGE_CURVE('',#4762,#4761,#4114,.T.);
#5788=EDGE_CURVE('',#4762,#4763,#2935,.T.);
#5789=EDGE_CURVE('',#4763,#4763,#4115,.T.);
#5790=EDGE_CURVE('',#4764,#4762,#4116,.T.);
#5791=EDGE_CURVE('',#4760,#4764,#2936,.T.);
#5792=EDGE_CURVE('',#4765,#4766,#2937,.T.);
#5793=EDGE_CURVE('',#4765,#4766,#4117,.T.);
#5794=EDGE_CURVE('',#4767,#4765,#2938,.T.);
#5795=EDGE_CURVE('',#4768,#4767,#4118,.T.);
#5796=EDGE_CURVE('',#4768,#4769,#2939,.T.);
#5797=EDGE_CURVE('',#4769,#4769,#4119,.T.);
#5798=EDGE_CURVE('',#4770,#4768,#4120,.T.);
#5799=EDGE_CURVE('',#4766,#4770,#2940,.T.);
#5800=EDGE_CURVE('',#4771,#4772,#2941,.T.);
#5801=EDGE_CURVE('',#4771,#4772,#4121,.T.);
#5802=EDGE_CURVE('',#4773,#4771,#2942,.T.);
#5803=EDGE_CURVE('',#4774,#4773,#4122,.T.);
#5804=EDGE_CURVE('',#4774,#4775,#2943,.T.);
#5805=EDGE_CURVE('',#4775,#4775,#4123,.T.);
#5806=EDGE_CURVE('',#4776,#4774,#4124,.T.);
#5807=EDGE_CURVE('',#4772,#4776,#2944,.T.);
#5808=EDGE_CURVE('',#4758,#4767,#2945,.T.);
#5809=EDGE_CURVE('',#4770,#4777,#2946,.T.);
#5810=EDGE_CURVE('',#4778,#4777,#2947,.T.);
#5811=EDGE_CURVE('',#4778,#4779,#2948,.T.);
#5812=EDGE_CURVE('',#4780,#4779,#2949,.T.);
#5813=EDGE_CURVE('',#4780,#4755,#2950,.T.);
#5814=EDGE_CURVE('',#4764,#4773,#2951,.T.);
#5815=EDGE_CURVE('',#4776,#4781,#2952,.T.);
#5816=EDGE_CURVE('',#4782,#4781,#2953,.T.);
#5817=EDGE_CURVE('',#4783,#4782,#2954,.T.);
#5818=EDGE_CURVE('',#4784,#4783,#2955,.T.);
#5819=EDGE_CURVE('',#4784,#4761,#2956,.T.);
#5820=EDGE_CURVE('',#4777,#4785,#2957,.T.);
#5821=EDGE_CURVE('',#4785,#4786,#2958,.T.);
#5822=EDGE_CURVE('',#4786,#4787,#2959,.T.);
#5823=EDGE_CURVE('',#4787,#4788,#2960,.T.);
#5824=EDGE_CURVE('',#4788,#4784,#2961,.T.);
#5825=EDGE_CURVE('',#4783,#4789,#2962,.T.);
#5826=EDGE_CURVE('',#4789,#4790,#2963,.T.);
#5827=EDGE_CURVE('',#4790,#4791,#2964,.T.);
#5828=EDGE_CURVE('',#4791,#4792,#2965,.T.);
#5829=EDGE_CURVE('',#4792,#4778,#2966,.T.);
#5830=EDGE_CURVE('',#4793,#4780,#2967,.T.);
#5831=EDGE_CURVE('',#4785,#4793,#2968,.T.);
#5832=EDGE_CURVE('',#4794,#4793,#2969,.T.);
#5833=EDGE_CURVE('',#4786,#4794,#2970,.T.);
#5834=EDGE_CURVE('',#4795,#4794,#2971,.T.);
#5835=EDGE_CURVE('',#4787,#4795,#2972,.T.);
#5836=EDGE_CURVE('',#4796,#4795,#2973,.T.);
#5837=EDGE_CURVE('',#4788,#4796,#2974,.T.);
#5838=EDGE_CURVE('',#4781,#4796,#2975,.T.);
#5839=EDGE_CURVE('',#4797,#4782,#2976,.T.);
#5840=EDGE_CURVE('',#4789,#4797,#2977,.T.);
#5841=EDGE_CURVE('',#4798,#4797,#2978,.T.);
#5842=EDGE_CURVE('',#4790,#4798,#2979,.T.);
#5843=EDGE_CURVE('',#4799,#4798,#2980,.T.);
#5844=EDGE_CURVE('',#4791,#4799,#2981,.T.);
#5845=EDGE_CURVE('',#4800,#4799,#2982,.T.);
#5846=EDGE_CURVE('',#4792,#4800,#2983,.T.);
#5847=EDGE_CURVE('',#4779,#4800,#2984,.T.);
#5848=EDGE_CURVE('',#4801,#4802,#2985,.T.);
#5849=EDGE_CURVE('',#4802,#4803,#2986,.T.);
#5850=EDGE_CURVE('',#4804,#4803,#2987,.T.);
#5851=EDGE_CURVE('',#4801,#4804,#2988,.T.);
#5852=EDGE_CURVE('',#4805,#4801,#2989,.T.);
#5853=EDGE_CURVE('',#4806,#4804,#2990,.T.);
#5854=EDGE_CURVE('',#4805,#4806,#2991,.T.);
#5855=EDGE_CURVE('',#4807,#4805,#2992,.T.);
#5856=EDGE_CURVE('',#4808,#4806,#2993,.T.);
#5857=EDGE_CURVE('',#4807,#4808,#2994,.T.);
#5858=EDGE_CURVE('',#4809,#4807,#2995,.T.);
#5859=EDGE_CURVE('',#4810,#4808,#2996,.T.);
#5860=EDGE_CURVE('',#4809,#4810,#2997,.T.);
#5861=EDGE_CURVE('',#4811,#4809,#2998,.T.);
#5862=EDGE_CURVE('',#4812,#4810,#2999,.T.);
#5863=EDGE_CURVE('',#4811,#4812,#3000,.T.);
#5864=EDGE_CURVE('',#4813,#4811,#3001,.T.);
#5865=EDGE_CURVE('',#4814,#4812,#3002,.T.);
#5866=EDGE_CURVE('',#4813,#4814,#3003,.T.);
#5867=EDGE_CURVE('',#4815,#4813,#3004,.T.);
#5868=EDGE_CURVE('',#4816,#4814,#3005,.T.);
#5869=EDGE_CURVE('',#4815,#4816,#3006,.T.);
#5870=EDGE_CURVE('',#4802,#4815,#3007,.T.);
#5871=EDGE_CURVE('',#4803,#4816,#3008,.T.);
#5872=EDGE_CURVE('',#4817,#4818,#3009,.T.);
#5873=EDGE_CURVE('',#4817,#4819,#3010,.T.);
#5874=EDGE_CURVE('',#4820,#4819,#3011,.T.);
#5875=EDGE_CURVE('',#4818,#4820,#3012,.T.);
#5876=EDGE_CURVE('',#4818,#4821,#3013,.T.);
#5877=EDGE_CURVE('',#4822,#4820,#3014,.T.);
#5878=EDGE_CURVE('',#4821,#4822,#3015,.T.);
#5879=EDGE_CURVE('',#4821,#4823,#3016,.T.);
#5880=EDGE_CURVE('',#4824,#4822,#3017,.T.);
#5881=EDGE_CURVE('',#4823,#4824,#3018,.T.);
#5882=EDGE_CURVE('',#4823,#4825,#3019,.T.);
#5883=EDGE_CURVE('',#4826,#4824,#3020,.T.);
#5884=EDGE_CURVE('',#4825,#4826,#3021,.T.);
#5885=EDGE_CURVE('',#4825,#4827,#3022,.T.);
#5886=EDGE_CURVE('',#4828,#4826,#3023,.T.);
#5887=EDGE_CURVE('',#4827,#4828,#3024,.T.);
#5888=EDGE_CURVE('',#4827,#4829,#3025,.T.);
#5889=EDGE_CURVE('',#4830,#4828,#3026,.T.);
#5890=EDGE_CURVE('',#4829,#4830,#3027,.T.);
#5891=EDGE_CURVE('',#4829,#4831,#3028,.T.);
#5892=EDGE_CURVE('',#4832,#4830,#3029,.T.);
#5893=EDGE_CURVE('',#4831,#4832,#3030,.T.);
#5894=EDGE_CURVE('',#4831,#4817,#3031,.T.);
#5895=EDGE_CURVE('',#4819,#4832,#3032,.T.);
#5896=EDGE_CURVE('',#4833,#4834,#3033,.T.);
#5897=EDGE_CURVE('',#4834,#4835,#3034,.T.);
#5898=EDGE_CURVE('',#4835,#4836,#3035,.T.);
#5899=EDGE_CURVE('',#4833,#4836,#3036,.T.);
#5900=EDGE_CURVE('',#4834,#4837,#3037,.T.);
#5901=EDGE_CURVE('',#4837,#4838,#3038,.T.);
#5902=EDGE_CURVE('',#4838,#4835,#3039,.T.);
#5903=EDGE_CURVE('',#4837,#4839,#3040,.T.);
#5904=EDGE_CURVE('',#4839,#4840,#3041,.T.);
#5905=EDGE_CURVE('',#4840,#4838,#3042,.T.);
#5906=EDGE_CURVE('',#4839,#4841,#3043,.T.);
#5907=EDGE_CURVE('',#4841,#4842,#3044,.T.);
#5908=EDGE_CURVE('',#4842,#4840,#3045,.T.);
#5909=EDGE_CURVE('',#4841,#4843,#3046,.T.);
#5910=EDGE_CURVE('',#4843,#4844,#3047,.T.);
#5911=EDGE_CURVE('',#4844,#4842,#3048,.T.);
#5912=EDGE_CURVE('',#4843,#4833,#3049,.T.);
#5913=EDGE_CURVE('',#4836,#4844,#3050,.T.);
#5914=EDGE_CURVE('',#4845,#4845,#4125,.T.);
#5915=EDGE_CURVE('',#4846,#4846,#4126,.T.);
#5916=EDGE_CURVE('',#4847,#4847,#4127,.T.);
#5917=EDGE_CURVE('',#4847,#4846,#3051,.T.);
#5918=EDGE_CURVE('',#4848,#4848,#4128,.T.);
#5919=EDGE_CURVE('',#4848,#4847,#3052,.T.);
#5920=EDGE_CURVE('',#4849,#4849,#4129,.T.);
#5921=EDGE_CURVE('',#4849,#4848,#3053,.T.);
#5922=EDGE_CURVE('',#4850,#4850,#4130,.T.);
#5923=EDGE_CURVE('',#4851,#4851,#4131,.F.);
#5924=EDGE_CURVE('',#4851,#4850,#3054,.T.);
#5925=EDGE_CURVE('',#4845,#4851,#3055,.T.);
#5926=EDGE_CURVE('',#4852,#4852,#4132,.T.);
#5927=EDGE_CURVE('',#4852,#4853,#3056,.T.);
#5928=EDGE_CURVE('',#4853,#4853,#4133,.T.);
#5929=EDGE_CURVE('',#4853,#4854,#3057,.T.);
#5930=EDGE_CURVE('',#4854,#4854,#4134,.T.);
#5931=EDGE_CURVE('',#4855,#4855,#4135,.T.);
#5932=EDGE_CURVE('',#4855,#4856,#3058,.T.);
#5933=EDGE_CURVE('',#4856,#4856,#4136,.T.);
#5934=EDGE_CURVE('',#4857,#4857,#4137,.T.);
#5935=EDGE_CURVE('',#4858,#4858,#4138,.T.);
#5936=EDGE_CURVE('',#4858,#4857,#3059,.T.);
#5937=EDGE_CURVE('',#4859,#4859,#4139,.T.);
#5938=EDGE_CURVE('',#4859,#4858,#3060,.T.);
#5939=EDGE_CURVE('',#4860,#4860,#4140,.T.);
#5940=EDGE_CURVE('',#4860,#4859,#3061,.T.);
#5941=EDGE_CURVE('',#4861,#4861,#4141,.T.);
#5942=EDGE_CURVE('',#4862,#4862,#4142,.F.);
#5943=EDGE_CURVE('',#4862,#4861,#3062,.T.);
#5944=EDGE_CURVE('',#4863,#4863,#4143,.F.);
#5945=EDGE_CURVE('',#4863,#4862,#3063,.T.);
#5946=EDGE_CURVE('',#4864,#4864,#4144,.T.);
#5947=EDGE_CURVE('',#4864,#4863,#3064,.T.);
#5948=EDGE_CURVE('',#4865,#4866,#3065,.T.);
#5949=EDGE_CURVE('',#4866,#4867,#3066,.T.);
#5950=EDGE_CURVE('',#4867,#4868,#3067,.T.);
#5951=EDGE_CURVE('',#4865,#4868,#3068,.T.);
#5952=EDGE_CURVE('',#4866,#4869,#3069,.T.);
#5953=EDGE_CURVE('',#4869,#4870,#3070,.T.);
#5954=EDGE_CURVE('',#4870,#4867,#3071,.T.);
#5955=EDGE_CURVE('',#4869,#4871,#3072,.T.);
#5956=EDGE_CURVE('',#4871,#4872,#3073,.T.);
#5957=EDGE_CURVE('',#4872,#4870,#3074,.T.);
#5958=EDGE_CURVE('',#4871,#4873,#3075,.T.);
#5959=EDGE_CURVE('',#4873,#4874,#3076,.T.);
#5960=EDGE_CURVE('',#4874,#4872,#3077,.T.);
#5961=EDGE_CURVE('',#4873,#4875,#3078,.T.);
#5962=EDGE_CURVE('',#4875,#4876,#3079,.T.);
#5963=EDGE_CURVE('',#4876,#4874,#3080,.T.);
#5964=EDGE_CURVE('',#4875,#4865,#3081,.T.);
#5965=EDGE_CURVE('',#4868,#4876,#3082,.T.);
#5966=EDGE_CURVE('',#4877,#4878,#3083,.T.);
#5967=EDGE_CURVE('',#4878,#4879,#3084,.T.);
#5968=EDGE_CURVE('',#4879,#4880,#3085,.T.);
#5969=EDGE_CURVE('',#4877,#4880,#3086,.T.);
#5970=EDGE_CURVE('',#4878,#4881,#3087,.T.);
#5971=EDGE_CURVE('',#4881,#4882,#3088,.T.);
#5972=EDGE_CURVE('',#4882,#4879,#3089,.T.);
#5973=EDGE_CURVE('',#4881,#4883,#3090,.T.);
#5974=EDGE_CURVE('',#4883,#4884,#3091,.T.);
#5975=EDGE_CURVE('',#4884,#4882,#3092,.T.);
#5976=EDGE_CURVE('',#4883,#4885,#3093,.T.);
#5977=EDGE_CURVE('',#4885,#4886,#3094,.T.);
#5978=EDGE_CURVE('',#4886,#4884,#3095,.T.);
#5979=EDGE_CURVE('',#4885,#4887,#3096,.T.);
#5980=EDGE_CURVE('',#4887,#4888,#3097,.T.);
#5981=EDGE_CURVE('',#4888,#4886,#3098,.T.);
#5982=EDGE_CURVE('',#4887,#4877,#3099,.T.);
#5983=EDGE_CURVE('',#4880,#4888,#3100,.T.);
#5984=EDGE_CURVE('',#4889,#4889,#4145,.T.);
#5985=EDGE_CURVE('',#4890,#4890,#4146,.T.);
#5986=EDGE_CURVE('',#4891,#4891,#4147,.T.);
#5987=EDGE_CURVE('',#4891,#4890,#3101,.T.);
#5988=EDGE_CURVE('',#4892,#4892,#4148,.T.);
#5989=EDGE_CURVE('',#4892,#4891,#3102,.T.);
#5990=EDGE_CURVE('',#4893,#4893,#4149,.T.);
#5991=EDGE_CURVE('',#4893,#4892,#3103,.T.);
#5992=EDGE_CURVE('',#4894,#4894,#4150,.T.);
#5993=EDGE_CURVE('',#4895,#4895,#4151,.F.);
#5994=EDGE_CURVE('',#4895,#4894,#3104,.T.);
#5995=EDGE_CURVE('',#4889,#4895,#3105,.T.);
#5996=ORIENTED_EDGE('',*,*,#4896,.F.);
#5997=ORIENTED_EDGE('',*,*,#4897,.T.);
#5998=ORIENTED_EDGE('',*,*,#4898,.F.);
#5999=ORIENTED_EDGE('',*,*,#4897,.F.);
#6000=ORIENTED_EDGE('',*,*,#4899,.F.);
#6001=ORIENTED_EDGE('',*,*,#4900,.T.);
#6002=ORIENTED_EDGE('',*,*,#4901,.F.);
#6003=ORIENTED_EDGE('',*,*,#4900,.F.);
#6004=ORIENTED_EDGE('',*,*,#4902,.F.);
#6005=ORIENTED_EDGE('',*,*,#4903,.T.);
#6006=ORIENTED_EDGE('',*,*,#4904,.F.);
#6007=ORIENTED_EDGE('',*,*,#4903,.F.);
#6008=ORIENTED_EDGE('',*,*,#4905,.F.);
#6009=ORIENTED_EDGE('',*,*,#4906,.T.);
#6010=ORIENTED_EDGE('',*,*,#4907,.F.);
#6011=ORIENTED_EDGE('',*,*,#4906,.F.);
#6012=ORIENTED_EDGE('',*,*,#4908,.F.);
#6013=ORIENTED_EDGE('',*,*,#4909,.T.);
#6014=ORIENTED_EDGE('',*,*,#4910,.F.);
#6015=ORIENTED_EDGE('',*,*,#4909,.F.);
#6016=ORIENTED_EDGE('',*,*,#4911,.F.);
#6017=ORIENTED_EDGE('',*,*,#4912,.T.);
#6018=ORIENTED_EDGE('',*,*,#4913,.F.);
#6019=ORIENTED_EDGE('',*,*,#4912,.F.);
#6020=ORIENTED_EDGE('',*,*,#4914,.F.);
#6021=ORIENTED_EDGE('',*,*,#4915,.T.);
#6022=ORIENTED_EDGE('',*,*,#4916,.F.);
#6023=ORIENTED_EDGE('',*,*,#4915,.F.);
#6024=ORIENTED_EDGE('',*,*,#4917,.F.);
#6025=ORIENTED_EDGE('',*,*,#4918,.T.);
#6026=ORIENTED_EDGE('',*,*,#4919,.F.);
#6027=ORIENTED_EDGE('',*,*,#4918,.F.);
#6028=ORIENTED_EDGE('',*,*,#4920,.F.);
#6029=ORIENTED_EDGE('',*,*,#4921,.T.);
#6030=ORIENTED_EDGE('',*,*,#4922,.F.);
#6031=ORIENTED_EDGE('',*,*,#4921,.F.);
#6032=ORIENTED_EDGE('',*,*,#4923,.F.);
#6033=ORIENTED_EDGE('',*,*,#4924,.T.);
#6034=ORIENTED_EDGE('',*,*,#4925,.F.);
#6035=ORIENTED_EDGE('',*,*,#4924,.F.);
#6036=ORIENTED_EDGE('',*,*,#4926,.F.);
#6037=ORIENTED_EDGE('',*,*,#4927,.T.);
#6038=ORIENTED_EDGE('',*,*,#4928,.F.);
#6039=ORIENTED_EDGE('',*,*,#4927,.F.);
#6040=ORIENTED_EDGE('',*,*,#4929,.F.);
#6041=ORIENTED_EDGE('',*,*,#4930,.T.);
#6042=ORIENTED_EDGE('',*,*,#4931,.F.);
#6043=ORIENTED_EDGE('',*,*,#4930,.F.);
#6044=ORIENTED_EDGE('',*,*,#4932,.T.);
#6045=ORIENTED_EDGE('',*,*,#4933,.T.);
#6046=ORIENTED_EDGE('',*,*,#4934,.F.);
#6047=ORIENTED_EDGE('',*,*,#4935,.F.);
#6048=ORIENTED_EDGE('',*,*,#4936,.T.);
#6049=ORIENTED_EDGE('',*,*,#4935,.T.);
#6050=ORIENTED_EDGE('',*,*,#4937,.F.);
#6051=ORIENTED_EDGE('',*,*,#4938,.F.);
#6052=ORIENTED_EDGE('',*,*,#4939,.T.);
#6053=ORIENTED_EDGE('',*,*,#4938,.T.);
#6054=ORIENTED_EDGE('',*,*,#4940,.F.);
#6055=ORIENTED_EDGE('',*,*,#4941,.F.);
#6056=ORIENTED_EDGE('',*,*,#4942,.T.);
#6057=ORIENTED_EDGE('',*,*,#4941,.T.);
#6058=ORIENTED_EDGE('',*,*,#4943,.F.);
#6059=ORIENTED_EDGE('',*,*,#4933,.F.);
#6060=ORIENTED_EDGE('',*,*,#4943,.T.);
#6061=ORIENTED_EDGE('',*,*,#4940,.T.);
#6062=ORIENTED_EDGE('',*,*,#4937,.T.);
#6063=ORIENTED_EDGE('',*,*,#4934,.T.);
#6064=ORIENTED_EDGE('',*,*,#4910,.T.);
#6065=ORIENTED_EDGE('',*,*,#4913,.T.);
#6066=ORIENTED_EDGE('',*,*,#4916,.T.);
#6067=ORIENTED_EDGE('',*,*,#4919,.T.);
#6068=ORIENTED_EDGE('',*,*,#4922,.T.);
#6069=ORIENTED_EDGE('',*,*,#4925,.T.);
#6070=ORIENTED_EDGE('',*,*,#4928,.T.);
#6071=ORIENTED_EDGE('',*,*,#4931,.T.);
#6072=ORIENTED_EDGE('',*,*,#4907,.T.);
#6073=ORIENTED_EDGE('',*,*,#4904,.T.);
#6074=ORIENTED_EDGE('',*,*,#4901,.T.);
#6075=ORIENTED_EDGE('',*,*,#4898,.T.);
#6076=ORIENTED_EDGE('',*,*,#4942,.F.);
#6077=ORIENTED_EDGE('',*,*,#4932,.F.);
#6078=ORIENTED_EDGE('',*,*,#4936,.F.);
#6079=ORIENTED_EDGE('',*,*,#4939,.F.);
#6080=ORIENTED_EDGE('',*,*,#4908,.T.);
#6081=ORIENTED_EDGE('',*,*,#4911,.T.);
#6082=ORIENTED_EDGE('',*,*,#4914,.T.);
#6083=ORIENTED_EDGE('',*,*,#4917,.T.);
#6084=ORIENTED_EDGE('',*,*,#4920,.T.);
#6085=ORIENTED_EDGE('',*,*,#4923,.T.);
#6086=ORIENTED_EDGE('',*,*,#4926,.T.);
#6087=ORIENTED_EDGE('',*,*,#4929,.T.);
#6088=ORIENTED_EDGE('',*,*,#4905,.T.);
#6089=ORIENTED_EDGE('',*,*,#4902,.T.);
#6090=ORIENTED_EDGE('',*,*,#4899,.T.);
#6091=ORIENTED_EDGE('',*,*,#4896,.T.);
#6092=ORIENTED_EDGE('',*,*,#4944,.F.);
#6093=ORIENTED_EDGE('',*,*,#4945,.T.);
#6094=ORIENTED_EDGE('',*,*,#4946,.F.);
#6095=ORIENTED_EDGE('',*,*,#4945,.F.);
#6096=ORIENTED_EDGE('',*,*,#4944,.T.);
#6097=ORIENTED_EDGE('',*,*,#4947,.F.);
#6098=ORIENTED_EDGE('',*,*,#4948,.T.);
#6099=ORIENTED_EDGE('',*,*,#4949,.F.);
#6100=ORIENTED_EDGE('',*,*,#4948,.F.);
#6101=ORIENTED_EDGE('',*,*,#4947,.T.);
#6102=ORIENTED_EDGE('',*,*,#4950,.F.);
#6103=ORIENTED_EDGE('',*,*,#4951,.T.);
#6104=ORIENTED_EDGE('',*,*,#4952,.F.);
#6105=ORIENTED_EDGE('',*,*,#4951,.F.);
#6106=ORIENTED_EDGE('',*,*,#4950,.T.);
#6107=ORIENTED_EDGE('',*,*,#4953,.F.);
#6108=ORIENTED_EDGE('',*,*,#4954,.F.);
#6109=ORIENTED_EDGE('',*,*,#4955,.T.);
#6110=ORIENTED_EDGE('',*,*,#4956,.F.);
#6111=ORIENTED_EDGE('',*,*,#4955,.F.);
#6112=ORIENTED_EDGE('',*,*,#4954,.T.);
#6113=ORIENTED_EDGE('',*,*,#4957,.F.);
#6114=ORIENTED_EDGE('',*,*,#4958,.F.);
#6115=ORIENTED_EDGE('',*,*,#4959,.T.);
#6116=ORIENTED_EDGE('',*,*,#4960,.F.);
#6117=ORIENTED_EDGE('',*,*,#4959,.F.);
#6118=ORIENTED_EDGE('',*,*,#4958,.T.);
#6119=ORIENTED_EDGE('',*,*,#4961,.F.);
#6120=ORIENTED_EDGE('',*,*,#4962,.F.);
#6121=ORIENTED_EDGE('',*,*,#4963,.T.);
#6122=ORIENTED_EDGE('',*,*,#4964,.F.);
#6123=ORIENTED_EDGE('',*,*,#4963,.F.);
#6124=ORIENTED_EDGE('',*,*,#4962,.T.);
#6125=ORIENTED_EDGE('',*,*,#4965,.F.);
#6126=ORIENTED_EDGE('',*,*,#4966,.F.);
#6127=ORIENTED_EDGE('',*,*,#4967,.T.);
#6128=ORIENTED_EDGE('',*,*,#4953,.T.);
#6129=ORIENTED_EDGE('',*,*,#4967,.F.);
#6130=ORIENTED_EDGE('',*,*,#4968,.F.);
#6131=ORIENTED_EDGE('',*,*,#4969,.T.);
#6132=ORIENTED_EDGE('',*,*,#4957,.T.);
#6133=ORIENTED_EDGE('',*,*,#4969,.F.);
#6134=ORIENTED_EDGE('',*,*,#4970,.F.);
#6135=ORIENTED_EDGE('',*,*,#4971,.T.);
#6136=ORIENTED_EDGE('',*,*,#4961,.T.);
#6137=ORIENTED_EDGE('',*,*,#4971,.F.);
#6138=ORIENTED_EDGE('',*,*,#4972,.F.);
#6139=ORIENTED_EDGE('',*,*,#4973,.T.);
#6140=ORIENTED_EDGE('',*,*,#4965,.T.);
#6141=ORIENTED_EDGE('',*,*,#4973,.F.);
#6142=ORIENTED_EDGE('',*,*,#4974,.T.);
#6143=ORIENTED_EDGE('',*,*,#4975,.T.);
#6144=ORIENTED_EDGE('',*,*,#4976,.F.);
#6145=ORIENTED_EDGE('',*,*,#4977,.F.);
#6146=ORIENTED_EDGE('',*,*,#4978,.T.);
#6147=ORIENTED_EDGE('',*,*,#4977,.T.);
#6148=ORIENTED_EDGE('',*,*,#4979,.F.);
#6149=ORIENTED_EDGE('',*,*,#4980,.F.);
#6150=ORIENTED_EDGE('',*,*,#4981,.T.);
#6151=ORIENTED_EDGE('',*,*,#4980,.T.);
#6152=ORIENTED_EDGE('',*,*,#4982,.F.);
#6153=ORIENTED_EDGE('',*,*,#4983,.F.);
#6154=ORIENTED_EDGE('',*,*,#4984,.T.);
#6155=ORIENTED_EDGE('',*,*,#4983,.T.);
#6156=ORIENTED_EDGE('',*,*,#4985,.F.);
#6157=ORIENTED_EDGE('',*,*,#4975,.F.);
#6158=ORIENTED_EDGE('',*,*,#4985,.T.);
#6159=ORIENTED_EDGE('',*,*,#4982,.T.);
#6160=ORIENTED_EDGE('',*,*,#4979,.T.);
#6161=ORIENTED_EDGE('',*,*,#4976,.T.);
#6162=ORIENTED_EDGE('',*,*,#4946,.T.);
#6163=ORIENTED_EDGE('',*,*,#4949,.T.);
#6164=ORIENTED_EDGE('',*,*,#4964,.T.);
#6165=ORIENTED_EDGE('',*,*,#4960,.T.);
#6166=ORIENTED_EDGE('',*,*,#4956,.T.);
#6167=ORIENTED_EDGE('',*,*,#4952,.T.);
#6168=ORIENTED_EDGE('',*,*,#4984,.F.);
#6169=ORIENTED_EDGE('',*,*,#4974,.F.);
#6170=ORIENTED_EDGE('',*,*,#4978,.F.);
#6171=ORIENTED_EDGE('',*,*,#4981,.F.);
#6172=ORIENTED_EDGE('',*,*,#4966,.T.);
#6173=ORIENTED_EDGE('',*,*,#4968,.T.);
#6174=ORIENTED_EDGE('',*,*,#4970,.T.);
#6175=ORIENTED_EDGE('',*,*,#4972,.T.);
#6176=ORIENTED_EDGE('',*,*,#4986,.F.);
#6177=ORIENTED_EDGE('',*,*,#4987,.T.);
#6178=ORIENTED_EDGE('',*,*,#4988,.T.);
#6179=ORIENTED_EDGE('',*,*,#4987,.F.);
#6180=ORIENTED_EDGE('',*,*,#4989,.F.);
#6181=ORIENTED_EDGE('',*,*,#4990,.T.);
#6182=ORIENTED_EDGE('',*,*,#4991,.T.);
#6183=ORIENTED_EDGE('',*,*,#4990,.F.);
#6184=ORIENTED_EDGE('',*,*,#4989,.T.);
#6185=ORIENTED_EDGE('',*,*,#4986,.T.);
#6186=ORIENTED_EDGE('',*,*,#4991,.F.);
#6187=ORIENTED_EDGE('',*,*,#4988,.F.);
#6188=ORIENTED_EDGE('',*,*,#4992,.F.);
#6189=ORIENTED_EDGE('',*,*,#4993,.T.);
#6190=ORIENTED_EDGE('',*,*,#4994,.T.);
#6191=ORIENTED_EDGE('',*,*,#4993,.F.);
#6192=ORIENTED_EDGE('',*,*,#4995,.F.);
#6193=ORIENTED_EDGE('',*,*,#4996,.T.);
#6194=ORIENTED_EDGE('',*,*,#4997,.T.);
#6195=ORIENTED_EDGE('',*,*,#4996,.F.);
#6196=ORIENTED_EDGE('',*,*,#4995,.T.);
#6197=ORIENTED_EDGE('',*,*,#4992,.T.);
#6198=ORIENTED_EDGE('',*,*,#4997,.F.);
#6199=ORIENTED_EDGE('',*,*,#4994,.F.);
#6200=ORIENTED_EDGE('',*,*,#4998,.F.);
#6201=ORIENTED_EDGE('',*,*,#4999,.T.);
#6202=ORIENTED_EDGE('',*,*,#5000,.F.);
#6203=ORIENTED_EDGE('',*,*,#4999,.F.);
#6204=ORIENTED_EDGE('',*,*,#4998,.T.);
#6205=ORIENTED_EDGE('',*,*,#5001,.F.);
#6206=ORIENTED_EDGE('',*,*,#5002,.T.);
#6207=ORIENTED_EDGE('',*,*,#5003,.F.);
#6208=ORIENTED_EDGE('',*,*,#5002,.F.);
#6209=ORIENTED_EDGE('',*,*,#5001,.T.);
#6210=ORIENTED_EDGE('',*,*,#5004,.F.);
#6211=ORIENTED_EDGE('',*,*,#5005,.T.);
#6212=ORIENTED_EDGE('',*,*,#5006,.F.);
#6213=ORIENTED_EDGE('',*,*,#5005,.F.);
#6214=ORIENTED_EDGE('',*,*,#5004,.T.);
#6215=ORIENTED_EDGE('',*,*,#5007,.F.);
#6216=ORIENTED_EDGE('',*,*,#5008,.F.);
#6217=ORIENTED_EDGE('',*,*,#5009,.T.);
#6218=ORIENTED_EDGE('',*,*,#5010,.F.);
#6219=ORIENTED_EDGE('',*,*,#5009,.F.);
#6220=ORIENTED_EDGE('',*,*,#5008,.T.);
#6221=ORIENTED_EDGE('',*,*,#5011,.F.);
#6222=ORIENTED_EDGE('',*,*,#5012,.F.);
#6223=ORIENTED_EDGE('',*,*,#5013,.T.);
#6224=ORIENTED_EDGE('',*,*,#5014,.F.);
#6225=ORIENTED_EDGE('',*,*,#5013,.F.);
#6226=ORIENTED_EDGE('',*,*,#5012,.T.);
#6227=ORIENTED_EDGE('',*,*,#5015,.F.);
#6228=ORIENTED_EDGE('',*,*,#5016,.F.);
#6229=ORIENTED_EDGE('',*,*,#5017,.T.);
#6230=ORIENTED_EDGE('',*,*,#5018,.F.);
#6231=ORIENTED_EDGE('',*,*,#5017,.F.);
#6232=ORIENTED_EDGE('',*,*,#5016,.T.);
#6233=ORIENTED_EDGE('',*,*,#5019,.F.);
#6234=ORIENTED_EDGE('',*,*,#5020,.F.);
#6235=ORIENTED_EDGE('',*,*,#5021,.T.);
#6236=ORIENTED_EDGE('',*,*,#5007,.T.);
#6237=ORIENTED_EDGE('',*,*,#5021,.F.);
#6238=ORIENTED_EDGE('',*,*,#5022,.F.);
#6239=ORIENTED_EDGE('',*,*,#5023,.T.);
#6240=ORIENTED_EDGE('',*,*,#5011,.T.);
#6241=ORIENTED_EDGE('',*,*,#5023,.F.);
#6242=ORIENTED_EDGE('',*,*,#5024,.F.);
#6243=ORIENTED_EDGE('',*,*,#5025,.T.);
#6244=ORIENTED_EDGE('',*,*,#5015,.T.);
#6245=ORIENTED_EDGE('',*,*,#5025,.F.);
#6246=ORIENTED_EDGE('',*,*,#5026,.F.);
#6247=ORIENTED_EDGE('',*,*,#5027,.T.);
#6248=ORIENTED_EDGE('',*,*,#5019,.T.);
#6249=ORIENTED_EDGE('',*,*,#5027,.F.);
#6250=ORIENTED_EDGE('',*,*,#5028,.T.);
#6251=ORIENTED_EDGE('',*,*,#5029,.T.);
#6252=ORIENTED_EDGE('',*,*,#5030,.F.);
#6253=ORIENTED_EDGE('',*,*,#5031,.F.);
#6254=ORIENTED_EDGE('',*,*,#5032,.T.);
#6255=ORIENTED_EDGE('',*,*,#5031,.T.);
#6256=ORIENTED_EDGE('',*,*,#5033,.F.);
#6257=ORIENTED_EDGE('',*,*,#5034,.F.);
#6258=ORIENTED_EDGE('',*,*,#5035,.T.);
#6259=ORIENTED_EDGE('',*,*,#5034,.T.);
#6260=ORIENTED_EDGE('',*,*,#5036,.F.);
#6261=ORIENTED_EDGE('',*,*,#5037,.F.);
#6262=ORIENTED_EDGE('',*,*,#5038,.T.);
#6263=ORIENTED_EDGE('',*,*,#5037,.T.);
#6264=ORIENTED_EDGE('',*,*,#5039,.F.);
#6265=ORIENTED_EDGE('',*,*,#5029,.F.);
#6266=ORIENTED_EDGE('',*,*,#5039,.T.);
#6267=ORIENTED_EDGE('',*,*,#5036,.T.);
#6268=ORIENTED_EDGE('',*,*,#5033,.T.);
#6269=ORIENTED_EDGE('',*,*,#5030,.T.);
#6270=ORIENTED_EDGE('',*,*,#5000,.T.);
#6271=ORIENTED_EDGE('',*,*,#5003,.T.);
#6272=ORIENTED_EDGE('',*,*,#5018,.T.);
#6273=ORIENTED_EDGE('',*,*,#5014,.T.);
#6274=ORIENTED_EDGE('',*,*,#5010,.T.);
#6275=ORIENTED_EDGE('',*,*,#5006,.T.);
#6276=ORIENTED_EDGE('',*,*,#5038,.F.);
#6277=ORIENTED_EDGE('',*,*,#5028,.F.);
#6278=ORIENTED_EDGE('',*,*,#5032,.F.);
#6279=ORIENTED_EDGE('',*,*,#5035,.F.);
#6280=ORIENTED_EDGE('',*,*,#5020,.T.);
#6281=ORIENTED_EDGE('',*,*,#5022,.T.);
#6282=ORIENTED_EDGE('',*,*,#5024,.T.);
#6283=ORIENTED_EDGE('',*,*,#5026,.T.);
#6284=ORIENTED_EDGE('',*,*,#5040,.F.);
#6285=ORIENTED_EDGE('',*,*,#5041,.T.);
#6286=ORIENTED_EDGE('',*,*,#5042,.T.);
#6287=ORIENTED_EDGE('',*,*,#5041,.F.);
#6288=ORIENTED_EDGE('',*,*,#5043,.F.);
#6289=ORIENTED_EDGE('',*,*,#5044,.T.);
#6290=ORIENTED_EDGE('',*,*,#5045,.T.);
#6291=ORIENTED_EDGE('',*,*,#5044,.F.);
#6292=ORIENTED_EDGE('',*,*,#5043,.T.);
#6293=ORIENTED_EDGE('',*,*,#5040,.T.);
#6294=ORIENTED_EDGE('',*,*,#5045,.F.);
#6295=ORIENTED_EDGE('',*,*,#5042,.F.);
#6296=ORIENTED_EDGE('',*,*,#5046,.F.);
#6297=ORIENTED_EDGE('',*,*,#5047,.T.);
#6298=ORIENTED_EDGE('',*,*,#5048,.T.);
#6299=ORIENTED_EDGE('',*,*,#5047,.F.);
#6300=ORIENTED_EDGE('',*,*,#5049,.F.);
#6301=ORIENTED_EDGE('',*,*,#5050,.T.);
#6302=ORIENTED_EDGE('',*,*,#5051,.T.);
#6303=ORIENTED_EDGE('',*,*,#5050,.F.);
#6304=ORIENTED_EDGE('',*,*,#5049,.T.);
#6305=ORIENTED_EDGE('',*,*,#5046,.T.);
#6306=ORIENTED_EDGE('',*,*,#5051,.F.);
#6307=ORIENTED_EDGE('',*,*,#5048,.F.);
#6308=ORIENTED_EDGE('',*,*,#5052,.F.);
#6309=ORIENTED_EDGE('',*,*,#5053,.T.);
#6310=ORIENTED_EDGE('',*,*,#5054,.F.);
#6311=ORIENTED_EDGE('',*,*,#5053,.F.);
#6312=ORIENTED_EDGE('',*,*,#5052,.T.);
#6313=ORIENTED_EDGE('',*,*,#5055,.F.);
#6314=ORIENTED_EDGE('',*,*,#5056,.T.);
#6315=ORIENTED_EDGE('',*,*,#5057,.F.);
#6316=ORIENTED_EDGE('',*,*,#5056,.F.);
#6317=ORIENTED_EDGE('',*,*,#5055,.T.);
#6318=ORIENTED_EDGE('',*,*,#5058,.F.);
#6319=ORIENTED_EDGE('',*,*,#5059,.T.);
#6320=ORIENTED_EDGE('',*,*,#5060,.F.);
#6321=ORIENTED_EDGE('',*,*,#5059,.F.);
#6322=ORIENTED_EDGE('',*,*,#5058,.T.);
#6323=ORIENTED_EDGE('',*,*,#5061,.F.);
#6324=ORIENTED_EDGE('',*,*,#5062,.T.);
#6325=ORIENTED_EDGE('',*,*,#5063,.F.);
#6326=ORIENTED_EDGE('',*,*,#5062,.F.);
#6327=ORIENTED_EDGE('',*,*,#5061,.T.);
#6328=ORIENTED_EDGE('',*,*,#5064,.F.);
#6329=ORIENTED_EDGE('',*,*,#5065,.T.);
#6330=ORIENTED_EDGE('',*,*,#5066,.F.);
#6331=ORIENTED_EDGE('',*,*,#5065,.F.);
#6332=ORIENTED_EDGE('',*,*,#5064,.T.);
#6333=ORIENTED_EDGE('',*,*,#5067,.F.);
#6334=ORIENTED_EDGE('',*,*,#5068,.F.);
#6335=ORIENTED_EDGE('',*,*,#5069,.T.);
#6336=ORIENTED_EDGE('',*,*,#5070,.F.);
#6337=ORIENTED_EDGE('',*,*,#5069,.F.);
#6338=ORIENTED_EDGE('',*,*,#5068,.T.);
#6339=ORIENTED_EDGE('',*,*,#5071,.F.);
#6340=ORIENTED_EDGE('',*,*,#5072,.F.);
#6341=ORIENTED_EDGE('',*,*,#5073,.T.);
#6342=ORIENTED_EDGE('',*,*,#5074,.F.);
#6343=ORIENTED_EDGE('',*,*,#5073,.F.);
#6344=ORIENTED_EDGE('',*,*,#5072,.T.);
#6345=ORIENTED_EDGE('',*,*,#5075,.F.);
#6346=ORIENTED_EDGE('',*,*,#5076,.F.);
#6347=ORIENTED_EDGE('',*,*,#5077,.T.);
#6348=ORIENTED_EDGE('',*,*,#5078,.F.);
#6349=ORIENTED_EDGE('',*,*,#5077,.F.);
#6350=ORIENTED_EDGE('',*,*,#5076,.T.);
#6351=ORIENTED_EDGE('',*,*,#5079,.F.);
#6352=ORIENTED_EDGE('',*,*,#5080,.F.);
#6353=ORIENTED_EDGE('',*,*,#5081,.T.);
#6354=ORIENTED_EDGE('',*,*,#5067,.T.);
#6355=ORIENTED_EDGE('',*,*,#5081,.F.);
#6356=ORIENTED_EDGE('',*,*,#5082,.F.);
#6357=ORIENTED_EDGE('',*,*,#5083,.T.);
#6358=ORIENTED_EDGE('',*,*,#5071,.T.);
#6359=ORIENTED_EDGE('',*,*,#5083,.F.);
#6360=ORIENTED_EDGE('',*,*,#5084,.F.);
#6361=ORIENTED_EDGE('',*,*,#5085,.T.);
#6362=ORIENTED_EDGE('',*,*,#5075,.T.);
#6363=ORIENTED_EDGE('',*,*,#5085,.F.);
#6364=ORIENTED_EDGE('',*,*,#5086,.F.);
#6365=ORIENTED_EDGE('',*,*,#5087,.T.);
#6366=ORIENTED_EDGE('',*,*,#5079,.T.);
#6367=ORIENTED_EDGE('',*,*,#5087,.F.);
#6368=ORIENTED_EDGE('',*,*,#5088,.T.);
#6369=ORIENTED_EDGE('',*,*,#5089,.T.);
#6370=ORIENTED_EDGE('',*,*,#5090,.F.);
#6371=ORIENTED_EDGE('',*,*,#5091,.F.);
#6372=ORIENTED_EDGE('',*,*,#5092,.T.);
#6373=ORIENTED_EDGE('',*,*,#5091,.T.);
#6374=ORIENTED_EDGE('',*,*,#5093,.F.);
#6375=ORIENTED_EDGE('',*,*,#5094,.F.);
#6376=ORIENTED_EDGE('',*,*,#5095,.T.);
#6377=ORIENTED_EDGE('',*,*,#5094,.T.);
#6378=ORIENTED_EDGE('',*,*,#5096,.F.);
#6379=ORIENTED_EDGE('',*,*,#5097,.F.);
#6380=ORIENTED_EDGE('',*,*,#5098,.T.);
#6381=ORIENTED_EDGE('',*,*,#5097,.T.);
#6382=ORIENTED_EDGE('',*,*,#5099,.F.);
#6383=ORIENTED_EDGE('',*,*,#5089,.F.);
#6384=ORIENTED_EDGE('',*,*,#5099,.T.);
#6385=ORIENTED_EDGE('',*,*,#5096,.T.);
#6386=ORIENTED_EDGE('',*,*,#5093,.T.);
#6387=ORIENTED_EDGE('',*,*,#5090,.T.);
#6388=ORIENTED_EDGE('',*,*,#5066,.T.);
#6389=ORIENTED_EDGE('',*,*,#5070,.T.);
#6390=ORIENTED_EDGE('',*,*,#5074,.T.);
#6391=ORIENTED_EDGE('',*,*,#5078,.T.);
#6392=ORIENTED_EDGE('',*,*,#5063,.T.);
#6393=ORIENTED_EDGE('',*,*,#5060,.T.);
#6394=ORIENTED_EDGE('',*,*,#5057,.T.);
#6395=ORIENTED_EDGE('',*,*,#5054,.T.);
#6396=ORIENTED_EDGE('',*,*,#5098,.F.);
#6397=ORIENTED_EDGE('',*,*,#5088,.F.);
#6398=ORIENTED_EDGE('',*,*,#5092,.F.);
#6399=ORIENTED_EDGE('',*,*,#5095,.F.);
#6400=ORIENTED_EDGE('',*,*,#5080,.T.);
#6401=ORIENTED_EDGE('',*,*,#5082,.T.);
#6402=ORIENTED_EDGE('',*,*,#5084,.T.);
#6403=ORIENTED_EDGE('',*,*,#5086,.T.);
#6404=ORIENTED_EDGE('',*,*,#5100,.T.);
#6405=ORIENTED_EDGE('',*,*,#5101,.T.);
#6406=ORIENTED_EDGE('',*,*,#5102,.F.);
#6407=ORIENTED_EDGE('',*,*,#5103,.F.);
#6408=ORIENTED_EDGE('',*,*,#5104,.T.);
#6409=ORIENTED_EDGE('',*,*,#5103,.T.);
#6410=ORIENTED_EDGE('',*,*,#5105,.F.);
#6411=ORIENTED_EDGE('',*,*,#5106,.F.);
#6412=ORIENTED_EDGE('',*,*,#5107,.T.);
#6413=ORIENTED_EDGE('',*,*,#5106,.T.);
#6414=ORIENTED_EDGE('',*,*,#5108,.F.);
#6415=ORIENTED_EDGE('',*,*,#5109,.F.);
#6416=ORIENTED_EDGE('',*,*,#5110,.T.);
#6417=ORIENTED_EDGE('',*,*,#5109,.T.);
#6418=ORIENTED_EDGE('',*,*,#5111,.F.);
#6419=ORIENTED_EDGE('',*,*,#5101,.F.);
#6420=ORIENTED_EDGE('',*,*,#5111,.T.);
#6421=ORIENTED_EDGE('',*,*,#5108,.T.);
#6422=ORIENTED_EDGE('',*,*,#5105,.T.);
#6423=ORIENTED_EDGE('',*,*,#5102,.T.);
#6424=ORIENTED_EDGE('',*,*,#5110,.F.);
#6425=ORIENTED_EDGE('',*,*,#5100,.F.);
#6426=ORIENTED_EDGE('',*,*,#5104,.F.);
#6427=ORIENTED_EDGE('',*,*,#5107,.F.);
#6428=ORIENTED_EDGE('',*,*,#5112,.T.);
#6429=ORIENTED_EDGE('',*,*,#5113,.T.);
#6430=ORIENTED_EDGE('',*,*,#5114,.F.);
#6431=ORIENTED_EDGE('',*,*,#5115,.F.);
#6432=ORIENTED_EDGE('',*,*,#5116,.T.);
#6433=ORIENTED_EDGE('',*,*,#5115,.T.);
#6434=ORIENTED_EDGE('',*,*,#5117,.F.);
#6435=ORIENTED_EDGE('',*,*,#5118,.F.);
#6436=ORIENTED_EDGE('',*,*,#5119,.T.);
#6437=ORIENTED_EDGE('',*,*,#5118,.T.);
#6438=ORIENTED_EDGE('',*,*,#5120,.F.);
#6439=ORIENTED_EDGE('',*,*,#5121,.F.);
#6440=ORIENTED_EDGE('',*,*,#5122,.T.);
#6441=ORIENTED_EDGE('',*,*,#5121,.T.);
#6442=ORIENTED_EDGE('',*,*,#5123,.F.);
#6443=ORIENTED_EDGE('',*,*,#5113,.F.);
#6444=ORIENTED_EDGE('',*,*,#5123,.T.);
#6445=ORIENTED_EDGE('',*,*,#5120,.T.);
#6446=ORIENTED_EDGE('',*,*,#5117,.T.);
#6447=ORIENTED_EDGE('',*,*,#5114,.T.);
#6448=ORIENTED_EDGE('',*,*,#5122,.F.);
#6449=ORIENTED_EDGE('',*,*,#5112,.F.);
#6450=ORIENTED_EDGE('',*,*,#5116,.F.);
#6451=ORIENTED_EDGE('',*,*,#5119,.F.);
#6452=ORIENTED_EDGE('',*,*,#5124,.F.);
#6453=ORIENTED_EDGE('',*,*,#5125,.T.);
#6454=ORIENTED_EDGE('',*,*,#5126,.F.);
#6455=ORIENTED_EDGE('',*,*,#5125,.F.);
#6456=ORIENTED_EDGE('',*,*,#5127,.F.);
#6457=ORIENTED_EDGE('',*,*,#5128,.T.);
#6458=ORIENTED_EDGE('',*,*,#5129,.F.);
#6459=ORIENTED_EDGE('',*,*,#5128,.F.);
#6460=ORIENTED_EDGE('',*,*,#5130,.T.);
#6461=ORIENTED_EDGE('',*,*,#5130,.F.);
#6462=ORIENTED_EDGE('',*,*,#5127,.T.);
#6463=ORIENTED_EDGE('',*,*,#5126,.T.);
#6464=ORIENTED_EDGE('',*,*,#5131,.F.);
#6465=ORIENTED_EDGE('',*,*,#5132,.T.);
#6466=ORIENTED_EDGE('',*,*,#5133,.F.);
#6467=ORIENTED_EDGE('',*,*,#5134,.F.);
#6468=ORIENTED_EDGE('',*,*,#5135,.F.);
#6469=ORIENTED_EDGE('',*,*,#5136,.T.);
#6470=ORIENTED_EDGE('',*,*,#5137,.F.);
#6471=ORIENTED_EDGE('',*,*,#5138,.F.);
#6472=ORIENTED_EDGE('',*,*,#5139,.T.);
#6473=ORIENTED_EDGE('',*,*,#5140,.F.);
#6474=ORIENTED_EDGE('',*,*,#5139,.F.);
#6475=ORIENTED_EDGE('',*,*,#5141,.F.);
#6476=ORIENTED_EDGE('',*,*,#5132,.F.);
#6477=ORIENTED_EDGE('',*,*,#5142,.F.);
#6478=ORIENTED_EDGE('',*,*,#5143,.T.);
#6479=ORIENTED_EDGE('',*,*,#5144,.F.);
#6480=ORIENTED_EDGE('',*,*,#5145,.F.);
#6481=ORIENTED_EDGE('',*,*,#5136,.F.);
#6482=ORIENTED_EDGE('',*,*,#5146,.F.);
#6483=ORIENTED_EDGE('',*,*,#5143,.F.);
#6484=ORIENTED_EDGE('',*,*,#5147,.T.);
#6485=ORIENTED_EDGE('',*,*,#5148,.T.);
#6486=ORIENTED_EDGE('',*,*,#5149,.T.);
#6487=ORIENTED_EDGE('',*,*,#5150,.T.);
#6488=ORIENTED_EDGE('',*,*,#5151,.T.);
#6489=ORIENTED_EDGE('',*,*,#5152,.T.);
#6490=ORIENTED_EDGE('',*,*,#5134,.T.);
#6491=ORIENTED_EDGE('',*,*,#5145,.T.);
#6492=ORIENTED_EDGE('',*,*,#5142,.T.);
#6493=ORIENTED_EDGE('',*,*,#5153,.T.);
#6494=ORIENTED_EDGE('',*,*,#5154,.T.);
#6495=ORIENTED_EDGE('',*,*,#5155,.T.);
#6496=ORIENTED_EDGE('',*,*,#5137,.T.);
#6497=ORIENTED_EDGE('',*,*,#5140,.T.);
#6498=ORIENTED_EDGE('',*,*,#5131,.T.);
#6499=ORIENTED_EDGE('',*,*,#5156,.T.);
#6500=ORIENTED_EDGE('',*,*,#5157,.T.);
#6501=ORIENTED_EDGE('',*,*,#5158,.T.);
#6502=ORIENTED_EDGE('',*,*,#5135,.T.);
#6503=ORIENTED_EDGE('',*,*,#5158,.F.);
#6504=ORIENTED_EDGE('',*,*,#5159,.F.);
#6505=ORIENTED_EDGE('',*,*,#5156,.F.);
#6506=ORIENTED_EDGE('',*,*,#5133,.T.);
#6507=ORIENTED_EDGE('',*,*,#5141,.T.);
#6508=ORIENTED_EDGE('',*,*,#5138,.T.);
#6509=ORIENTED_EDGE('',*,*,#5155,.F.);
#6510=ORIENTED_EDGE('',*,*,#5160,.F.);
#6511=ORIENTED_EDGE('',*,*,#5153,.F.);
#6512=ORIENTED_EDGE('',*,*,#5144,.T.);
#6513=ORIENTED_EDGE('',*,*,#5146,.T.);
#6514=ORIENTED_EDGE('',*,*,#5154,.F.);
#6515=ORIENTED_EDGE('',*,*,#5160,.T.);
#6516=ORIENTED_EDGE('',*,*,#5124,.T.);
#6517=ORIENTED_EDGE('',*,*,#5157,.F.);
#6518=ORIENTED_EDGE('',*,*,#5159,.T.);
#6519=ORIENTED_EDGE('',*,*,#5129,.T.);
#6520=ORIENTED_EDGE('',*,*,#5161,.F.);
#6521=ORIENTED_EDGE('',*,*,#5162,.T.);
#6522=ORIENTED_EDGE('',*,*,#5163,.T.);
#6523=ORIENTED_EDGE('',*,*,#5164,.F.);
#6524=ORIENTED_EDGE('',*,*,#5165,.F.);
#6525=ORIENTED_EDGE('',*,*,#5166,.T.);
#6526=ORIENTED_EDGE('',*,*,#5167,.T.);
#6527=ORIENTED_EDGE('',*,*,#5162,.F.);
#6528=ORIENTED_EDGE('',*,*,#5168,.F.);
#6529=ORIENTED_EDGE('',*,*,#5169,.T.);
#6530=ORIENTED_EDGE('',*,*,#5170,.T.);
#6531=ORIENTED_EDGE('',*,*,#5166,.F.);
#6532=ORIENTED_EDGE('',*,*,#5171,.F.);
#6533=ORIENTED_EDGE('',*,*,#5164,.T.);
#6534=ORIENTED_EDGE('',*,*,#5172,.T.);
#6535=ORIENTED_EDGE('',*,*,#5169,.F.);
#6536=ORIENTED_EDGE('',*,*,#5172,.F.);
#6537=ORIENTED_EDGE('',*,*,#5163,.F.);
#6538=ORIENTED_EDGE('',*,*,#5167,.F.);
#6539=ORIENTED_EDGE('',*,*,#5170,.F.);
#6540=ORIENTED_EDGE('',*,*,#5173,.F.);
#6541=ORIENTED_EDGE('',*,*,#5174,.T.);
#6542=ORIENTED_EDGE('',*,*,#5152,.F.);
#6543=ORIENTED_EDGE('',*,*,#5174,.F.);
#6544=ORIENTED_EDGE('',*,*,#5175,.F.);
#6545=ORIENTED_EDGE('',*,*,#5176,.T.);
#6546=ORIENTED_EDGE('',*,*,#5151,.F.);
#6547=ORIENTED_EDGE('',*,*,#5176,.F.);
#6548=ORIENTED_EDGE('',*,*,#5177,.T.);
#6549=ORIENTED_EDGE('',*,*,#5178,.T.);
#6550=ORIENTED_EDGE('',*,*,#5150,.F.);
#6551=ORIENTED_EDGE('',*,*,#5179,.F.);
#6552=ORIENTED_EDGE('',*,*,#5180,.T.);
#6553=ORIENTED_EDGE('',*,*,#5179,.T.);
#6554=ORIENTED_EDGE('',*,*,#5149,.F.);
#6555=ORIENTED_EDGE('',*,*,#5181,.F.);
#6556=ORIENTED_EDGE('',*,*,#5182,.T.);
#6557=ORIENTED_EDGE('',*,*,#5181,.T.);
#6558=ORIENTED_EDGE('',*,*,#5148,.F.);
#6559=ORIENTED_EDGE('',*,*,#5183,.F.);
#6560=ORIENTED_EDGE('',*,*,#5184,.T.);
#6561=ORIENTED_EDGE('',*,*,#5183,.T.);
#6562=ORIENTED_EDGE('',*,*,#5147,.F.);
#6563=ORIENTED_EDGE('',*,*,#5178,.F.);
#6564=ORIENTED_EDGE('',*,*,#5184,.F.);
#6565=ORIENTED_EDGE('',*,*,#5177,.F.);
#6566=ORIENTED_EDGE('',*,*,#5180,.F.);
#6567=ORIENTED_EDGE('',*,*,#5182,.F.);
#6568=ORIENTED_EDGE('',*,*,#5161,.T.);
#6569=ORIENTED_EDGE('',*,*,#5171,.T.);
#6570=ORIENTED_EDGE('',*,*,#5168,.T.);
#6571=ORIENTED_EDGE('',*,*,#5165,.T.);
#6572=ORIENTED_EDGE('',*,*,#5173,.T.);
#6573=ORIENTED_EDGE('',*,*,#5175,.T.);
#6574=ORIENTED_EDGE('',*,*,#5185,.T.);
#6575=ORIENTED_EDGE('',*,*,#5186,.T.);
#6576=ORIENTED_EDGE('',*,*,#5187,.F.);
#6577=ORIENTED_EDGE('',*,*,#5186,.F.);
#6578=ORIENTED_EDGE('',*,*,#5188,.F.);
#6579=ORIENTED_EDGE('',*,*,#5187,.T.);
#6580=ORIENTED_EDGE('',*,*,#5189,.T.);
#6581=ORIENTED_EDGE('',*,*,#5189,.F.);
#6582=ORIENTED_EDGE('',*,*,#5188,.T.);
#6583=ORIENTED_EDGE('',*,*,#5190,.F.);
#6584=ORIENTED_EDGE('',*,*,#5190,.T.);
#6585=ORIENTED_EDGE('',*,*,#5185,.F.);
#6586=ORIENTED_EDGE('',*,*,#5191,.F.);
#6587=ORIENTED_EDGE('',*,*,#5192,.F.);
#6588=ORIENTED_EDGE('',*,*,#5193,.F.);
#6589=ORIENTED_EDGE('',*,*,#5194,.T.);
#6590=ORIENTED_EDGE('',*,*,#5195,.F.);
#6591=ORIENTED_EDGE('',*,*,#5194,.F.);
#6592=ORIENTED_EDGE('',*,*,#5196,.F.);
#6593=ORIENTED_EDGE('',*,*,#5197,.T.);
#6594=ORIENTED_EDGE('',*,*,#5198,.F.);
#6595=ORIENTED_EDGE('',*,*,#5199,.F.);
#6596=ORIENTED_EDGE('',*,*,#5200,.F.);
#6597=ORIENTED_EDGE('',*,*,#5197,.F.);
#6598=ORIENTED_EDGE('',*,*,#5201,.F.);
#6599=ORIENTED_EDGE('',*,*,#5202,.T.);
#6600=ORIENTED_EDGE('',*,*,#5203,.T.);
#6601=ORIENTED_EDGE('',*,*,#5202,.F.);
#6602=ORIENTED_EDGE('',*,*,#5192,.T.);
#6603=ORIENTED_EDGE('',*,*,#5191,.T.);
#6604=ORIENTED_EDGE('',*,*,#5193,.T.);
#6605=ORIENTED_EDGE('',*,*,#5199,.T.);
#6606=ORIENTED_EDGE('',*,*,#5198,.T.);
#6607=ORIENTED_EDGE('',*,*,#5200,.T.);
#6608=ORIENTED_EDGE('',*,*,#5204,.T.);
#6609=ORIENTED_EDGE('',*,*,#5205,.T.);
#6610=ORIENTED_EDGE('',*,*,#5206,.T.);
#6611=ORIENTED_EDGE('',*,*,#5207,.T.);
#6612=ORIENTED_EDGE('',*,*,#5208,.T.);
#6613=ORIENTED_EDGE('',*,*,#5209,.T.);
#6614=ORIENTED_EDGE('',*,*,#5210,.T.);
#6615=ORIENTED_EDGE('',*,*,#5211,.T.);
#6616=ORIENTED_EDGE('',*,*,#5212,.T.);
#6617=ORIENTED_EDGE('',*,*,#5213,.T.);
#6618=ORIENTED_EDGE('',*,*,#5214,.T.);
#6619=ORIENTED_EDGE('',*,*,#5215,.T.);
#6620=ORIENTED_EDGE('',*,*,#5205,.F.);
#6621=ORIENTED_EDGE('',*,*,#5204,.F.);
#6622=ORIENTED_EDGE('',*,*,#5206,.F.);
#6623=ORIENTED_EDGE('',*,*,#5216,.T.);
#6624=ORIENTED_EDGE('',*,*,#5217,.F.);
#6625=ORIENTED_EDGE('',*,*,#5216,.F.);
#6626=ORIENTED_EDGE('',*,*,#5218,.F.);
#6627=ORIENTED_EDGE('',*,*,#5219,.T.);
#6628=ORIENTED_EDGE('',*,*,#5208,.F.);
#6629=ORIENTED_EDGE('',*,*,#5207,.F.);
#6630=ORIENTED_EDGE('',*,*,#5209,.F.);
#6631=ORIENTED_EDGE('',*,*,#5219,.F.);
#6632=ORIENTED_EDGE('',*,*,#5211,.F.);
#6633=ORIENTED_EDGE('',*,*,#5210,.F.);
#6634=ORIENTED_EDGE('',*,*,#5212,.F.);
#6635=ORIENTED_EDGE('',*,*,#5220,.T.);
#6636=ORIENTED_EDGE('',*,*,#5221,.F.);
#6637=ORIENTED_EDGE('',*,*,#5220,.F.);
#6638=ORIENTED_EDGE('',*,*,#5222,.F.);
#6639=ORIENTED_EDGE('',*,*,#5223,.T.);
#6640=ORIENTED_EDGE('',*,*,#5214,.F.);
#6641=ORIENTED_EDGE('',*,*,#5213,.F.);
#6642=ORIENTED_EDGE('',*,*,#5215,.F.);
#6643=ORIENTED_EDGE('',*,*,#5223,.F.);
#6644=ORIENTED_EDGE('',*,*,#5203,.F.);
#6645=ORIENTED_EDGE('',*,*,#5224,.T.);
#6646=ORIENTED_EDGE('',*,*,#5225,.F.);
#6647=ORIENTED_EDGE('',*,*,#5201,.T.);
#6648=ORIENTED_EDGE('',*,*,#5226,.F.);
#6649=ORIENTED_EDGE('',*,*,#5227,.T.);
#6650=ORIENTED_EDGE('',*,*,#5225,.T.);
#6651=ORIENTED_EDGE('',*,*,#5227,.F.);
#6652=ORIENTED_EDGE('',*,*,#5226,.T.);
#6653=ORIENTED_EDGE('',*,*,#5228,.F.);
#6654=ORIENTED_EDGE('',*,*,#5228,.T.);
#6655=ORIENTED_EDGE('',*,*,#5229,.T.);
#6656=ORIENTED_EDGE('',*,*,#5224,.F.);
#6657=ORIENTED_EDGE('',*,*,#5229,.F.);
#6658=ORIENTED_EDGE('',*,*,#5196,.T.);
#6659=ORIENTED_EDGE('',*,*,#5195,.T.);
#6660=ORIENTED_EDGE('',*,*,#5218,.T.);
#6661=ORIENTED_EDGE('',*,*,#5217,.T.);
#6662=ORIENTED_EDGE('',*,*,#5222,.T.);
#6663=ORIENTED_EDGE('',*,*,#5221,.T.);
#6664=ORIENTED_EDGE('',*,*,#5230,.F.);
#6665=ORIENTED_EDGE('',*,*,#5231,.T.);
#6666=ORIENTED_EDGE('',*,*,#5232,.T.);
#6667=ORIENTED_EDGE('',*,*,#5231,.F.);
#6668=ORIENTED_EDGE('',*,*,#5233,.F.);
#6669=ORIENTED_EDGE('',*,*,#5234,.T.);
#6670=ORIENTED_EDGE('',*,*,#5235,.T.);
#6671=ORIENTED_EDGE('',*,*,#5234,.F.);
#6672=ORIENTED_EDGE('',*,*,#5233,.T.);
#6673=ORIENTED_EDGE('',*,*,#5230,.T.);
#6674=ORIENTED_EDGE('',*,*,#5235,.F.);
#6675=ORIENTED_EDGE('',*,*,#5232,.F.);
#6676=ORIENTED_EDGE('',*,*,#5236,.T.);
#6677=ORIENTED_EDGE('',*,*,#5237,.T.);
#6678=ORIENTED_EDGE('',*,*,#5238,.T.);
#6679=ORIENTED_EDGE('',*,*,#5239,.F.);
#6680=ORIENTED_EDGE('',*,*,#5240,.T.);
#6681=ORIENTED_EDGE('',*,*,#5241,.T.);
#6682=ORIENTED_EDGE('',*,*,#5242,.T.);
#6683=ORIENTED_EDGE('',*,*,#5237,.F.);
#6684=ORIENTED_EDGE('',*,*,#5243,.T.);
#6685=ORIENTED_EDGE('',*,*,#5244,.T.);
#6686=ORIENTED_EDGE('',*,*,#5245,.T.);
#6687=ORIENTED_EDGE('',*,*,#5241,.F.);
#6688=ORIENTED_EDGE('',*,*,#5246,.T.);
#6689=ORIENTED_EDGE('',*,*,#5247,.T.);
#6690=ORIENTED_EDGE('',*,*,#5248,.T.);
#6691=ORIENTED_EDGE('',*,*,#5244,.F.);
#6692=ORIENTED_EDGE('',*,*,#5249,.T.);
#6693=ORIENTED_EDGE('',*,*,#5250,.T.);
#6694=ORIENTED_EDGE('',*,*,#5251,.T.);
#6695=ORIENTED_EDGE('',*,*,#5247,.F.);
#6696=ORIENTED_EDGE('',*,*,#5252,.T.);
#6697=ORIENTED_EDGE('',*,*,#5239,.T.);
#6698=ORIENTED_EDGE('',*,*,#5253,.T.);
#6699=ORIENTED_EDGE('',*,*,#5250,.F.);
#6700=ORIENTED_EDGE('',*,*,#5252,.F.);
#6701=ORIENTED_EDGE('',*,*,#5249,.F.);
#6702=ORIENTED_EDGE('',*,*,#5246,.F.);
#6703=ORIENTED_EDGE('',*,*,#5243,.F.);
#6704=ORIENTED_EDGE('',*,*,#5240,.F.);
#6705=ORIENTED_EDGE('',*,*,#5236,.F.);
#6706=ORIENTED_EDGE('',*,*,#5253,.F.);
#6707=ORIENTED_EDGE('',*,*,#5238,.F.);
#6708=ORIENTED_EDGE('',*,*,#5242,.F.);
#6709=ORIENTED_EDGE('',*,*,#5245,.F.);
#6710=ORIENTED_EDGE('',*,*,#5248,.F.);
#6711=ORIENTED_EDGE('',*,*,#5251,.F.);
#6712=ORIENTED_EDGE('',*,*,#5254,.F.);
#6713=ORIENTED_EDGE('',*,*,#5255,.F.);
#6714=ORIENTED_EDGE('',*,*,#5256,.F.);
#6715=ORIENTED_EDGE('',*,*,#5257,.T.);
#6716=ORIENTED_EDGE('',*,*,#5255,.T.);
#6717=ORIENTED_EDGE('',*,*,#5257,.F.);
#6718=ORIENTED_EDGE('',*,*,#5258,.F.);
#6719=ORIENTED_EDGE('',*,*,#5259,.T.);
#6720=ORIENTED_EDGE('',*,*,#5256,.T.);
#6721=ORIENTED_EDGE('',*,*,#5259,.F.);
#6722=ORIENTED_EDGE('',*,*,#5260,.F.);
#6723=ORIENTED_EDGE('',*,*,#5261,.T.);
#6724=ORIENTED_EDGE('',*,*,#5258,.T.);
#6725=ORIENTED_EDGE('',*,*,#5261,.F.);
#6726=ORIENTED_EDGE('',*,*,#5260,.T.);
#6727=ORIENTED_EDGE('',*,*,#5262,.F.);
#6728=ORIENTED_EDGE('',*,*,#5263,.F.);
#6729=ORIENTED_EDGE('',*,*,#5264,.T.);
#6730=ORIENTED_EDGE('',*,*,#5262,.T.);
#6731=ORIENTED_EDGE('',*,*,#5264,.F.);
#6732=ORIENTED_EDGE('',*,*,#5254,.T.);
#6733=ORIENTED_EDGE('',*,*,#5265,.T.);
#6734=ORIENTED_EDGE('',*,*,#5263,.T.);
#6735=ORIENTED_EDGE('',*,*,#5265,.F.);
#6736=ORIENTED_EDGE('',*,*,#5266,.F.);
#6737=ORIENTED_EDGE('',*,*,#5267,.T.);
#6738=ORIENTED_EDGE('',*,*,#5268,.F.);
#6739=ORIENTED_EDGE('',*,*,#5267,.F.);
#6740=ORIENTED_EDGE('',*,*,#5266,.T.);
#6741=ORIENTED_EDGE('',*,*,#5269,.F.);
#6742=ORIENTED_EDGE('',*,*,#5270,.F.);
#6743=ORIENTED_EDGE('',*,*,#5271,.T.);
#6744=ORIENTED_EDGE('',*,*,#5272,.F.);
#6745=ORIENTED_EDGE('',*,*,#5271,.F.);
#6746=ORIENTED_EDGE('',*,*,#5270,.T.);
#6747=ORIENTED_EDGE('',*,*,#5273,.F.);
#6748=ORIENTED_EDGE('',*,*,#5274,.F.);
#6749=ORIENTED_EDGE('',*,*,#5275,.T.);
#6750=ORIENTED_EDGE('',*,*,#5276,.F.);
#6751=ORIENTED_EDGE('',*,*,#5275,.F.);
#6752=ORIENTED_EDGE('',*,*,#5274,.T.);
#6753=ORIENTED_EDGE('',*,*,#5277,.F.);
#6754=ORIENTED_EDGE('',*,*,#5278,.F.);
#6755=ORIENTED_EDGE('',*,*,#5279,.T.);
#6756=ORIENTED_EDGE('',*,*,#5280,.F.);
#6757=ORIENTED_EDGE('',*,*,#5279,.F.);
#6758=ORIENTED_EDGE('',*,*,#5278,.T.);
#6759=ORIENTED_EDGE('',*,*,#5281,.F.);
#6760=ORIENTED_EDGE('',*,*,#5282,.F.);
#6761=ORIENTED_EDGE('',*,*,#5283,.T.);
#6762=ORIENTED_EDGE('',*,*,#5269,.T.);
#6763=ORIENTED_EDGE('',*,*,#5283,.F.);
#6764=ORIENTED_EDGE('',*,*,#5284,.F.);
#6765=ORIENTED_EDGE('',*,*,#5285,.T.);
#6766=ORIENTED_EDGE('',*,*,#5273,.T.);
#6767=ORIENTED_EDGE('',*,*,#5285,.F.);
#6768=ORIENTED_EDGE('',*,*,#5286,.F.);
#6769=ORIENTED_EDGE('',*,*,#5287,.T.);
#6770=ORIENTED_EDGE('',*,*,#5277,.T.);
#6771=ORIENTED_EDGE('',*,*,#5287,.F.);
#6772=ORIENTED_EDGE('',*,*,#5288,.F.);
#6773=ORIENTED_EDGE('',*,*,#5289,.T.);
#6774=ORIENTED_EDGE('',*,*,#5281,.T.);
#6775=ORIENTED_EDGE('',*,*,#5289,.F.);
#6776=ORIENTED_EDGE('',*,*,#5290,.T.);
#6777=ORIENTED_EDGE('',*,*,#5291,.T.);
#6778=ORIENTED_EDGE('',*,*,#5292,.F.);
#6779=ORIENTED_EDGE('',*,*,#5293,.F.);
#6780=ORIENTED_EDGE('',*,*,#5294,.T.);
#6781=ORIENTED_EDGE('',*,*,#5293,.T.);
#6782=ORIENTED_EDGE('',*,*,#5295,.F.);
#6783=ORIENTED_EDGE('',*,*,#5296,.F.);
#6784=ORIENTED_EDGE('',*,*,#5297,.T.);
#6785=ORIENTED_EDGE('',*,*,#5296,.T.);
#6786=ORIENTED_EDGE('',*,*,#5298,.F.);
#6787=ORIENTED_EDGE('',*,*,#5299,.F.);
#6788=ORIENTED_EDGE('',*,*,#5300,.T.);
#6789=ORIENTED_EDGE('',*,*,#5299,.T.);
#6790=ORIENTED_EDGE('',*,*,#5301,.F.);
#6791=ORIENTED_EDGE('',*,*,#5302,.F.);
#6792=ORIENTED_EDGE('',*,*,#5303,.T.);
#6793=ORIENTED_EDGE('',*,*,#5302,.T.);
#6794=ORIENTED_EDGE('',*,*,#5304,.F.);
#6795=ORIENTED_EDGE('',*,*,#5305,.F.);
#6796=ORIENTED_EDGE('',*,*,#5280,.T.);
#6797=ORIENTED_EDGE('',*,*,#5276,.T.);
#6798=ORIENTED_EDGE('',*,*,#5272,.T.);
#6799=ORIENTED_EDGE('',*,*,#5268,.T.);
#6800=ORIENTED_EDGE('',*,*,#5306,.T.);
#6801=ORIENTED_EDGE('',*,*,#5305,.T.);
#6802=ORIENTED_EDGE('',*,*,#5307,.F.);
#6803=ORIENTED_EDGE('',*,*,#5308,.F.);
#6804=ORIENTED_EDGE('',*,*,#5309,.T.);
#6805=ORIENTED_EDGE('',*,*,#5308,.T.);
#6806=ORIENTED_EDGE('',*,*,#5310,.F.);
#6807=ORIENTED_EDGE('',*,*,#5311,.F.);
#6808=ORIENTED_EDGE('',*,*,#5312,.T.);
#6809=ORIENTED_EDGE('',*,*,#5311,.T.);
#6810=ORIENTED_EDGE('',*,*,#5313,.F.);
#6811=ORIENTED_EDGE('',*,*,#5314,.F.);
#6812=ORIENTED_EDGE('',*,*,#5315,.T.);
#6813=ORIENTED_EDGE('',*,*,#5314,.T.);
#6814=ORIENTED_EDGE('',*,*,#5316,.F.);
#6815=ORIENTED_EDGE('',*,*,#5317,.F.);
#6816=ORIENTED_EDGE('',*,*,#5318,.T.);
#6817=ORIENTED_EDGE('',*,*,#5317,.T.);
#6818=ORIENTED_EDGE('',*,*,#5319,.F.);
#6819=ORIENTED_EDGE('',*,*,#5320,.F.);
#6820=ORIENTED_EDGE('',*,*,#5321,.T.);
#6821=ORIENTED_EDGE('',*,*,#5320,.T.);
#6822=ORIENTED_EDGE('',*,*,#5322,.F.);
#6823=ORIENTED_EDGE('',*,*,#5323,.F.);
#6824=ORIENTED_EDGE('',*,*,#5282,.T.);
#6825=ORIENTED_EDGE('',*,*,#5284,.T.);
#6826=ORIENTED_EDGE('',*,*,#5286,.T.);
#6827=ORIENTED_EDGE('',*,*,#5288,.T.);
#6828=ORIENTED_EDGE('',*,*,#5324,.T.);
#6829=ORIENTED_EDGE('',*,*,#5323,.T.);
#6830=ORIENTED_EDGE('',*,*,#5325,.F.);
#6831=ORIENTED_EDGE('',*,*,#5291,.F.);
#6832=ORIENTED_EDGE('',*,*,#5325,.T.);
#6833=ORIENTED_EDGE('',*,*,#5322,.T.);
#6834=ORIENTED_EDGE('',*,*,#5319,.T.);
#6835=ORIENTED_EDGE('',*,*,#5316,.T.);
#6836=ORIENTED_EDGE('',*,*,#5313,.T.);
#6837=ORIENTED_EDGE('',*,*,#5310,.T.);
#6838=ORIENTED_EDGE('',*,*,#5307,.T.);
#6839=ORIENTED_EDGE('',*,*,#5304,.T.);
#6840=ORIENTED_EDGE('',*,*,#5301,.T.);
#6841=ORIENTED_EDGE('',*,*,#5298,.T.);
#6842=ORIENTED_EDGE('',*,*,#5295,.T.);
#6843=ORIENTED_EDGE('',*,*,#5292,.T.);
#6844=ORIENTED_EDGE('',*,*,#5324,.F.);
#6845=ORIENTED_EDGE('',*,*,#5290,.F.);
#6846=ORIENTED_EDGE('',*,*,#5294,.F.);
#6847=ORIENTED_EDGE('',*,*,#5297,.F.);
#6848=ORIENTED_EDGE('',*,*,#5300,.F.);
#6849=ORIENTED_EDGE('',*,*,#5303,.F.);
#6850=ORIENTED_EDGE('',*,*,#5306,.F.);
#6851=ORIENTED_EDGE('',*,*,#5309,.F.);
#6852=ORIENTED_EDGE('',*,*,#5312,.F.);
#6853=ORIENTED_EDGE('',*,*,#5315,.F.);
#6854=ORIENTED_EDGE('',*,*,#5318,.F.);
#6855=ORIENTED_EDGE('',*,*,#5321,.F.);
#6856=ORIENTED_EDGE('',*,*,#5326,.F.);
#6857=ORIENTED_EDGE('',*,*,#5327,.F.);
#6858=ORIENTED_EDGE('',*,*,#5328,.T.);
#6859=ORIENTED_EDGE('',*,*,#5326,.T.);
#6860=ORIENTED_EDGE('',*,*,#5328,.F.);
#6861=ORIENTED_EDGE('',*,*,#5329,.F.);
#6862=ORIENTED_EDGE('',*,*,#5330,.T.);
#6863=ORIENTED_EDGE('',*,*,#5327,.T.);
#6864=ORIENTED_EDGE('',*,*,#5330,.F.);
#6865=ORIENTED_EDGE('',*,*,#5331,.F.);
#6866=ORIENTED_EDGE('',*,*,#5332,.T.);
#6867=ORIENTED_EDGE('',*,*,#5329,.T.);
#6868=ORIENTED_EDGE('',*,*,#5332,.F.);
#6869=ORIENTED_EDGE('',*,*,#5331,.T.);
#6870=ORIENTED_EDGE('',*,*,#5333,.F.);
#6871=ORIENTED_EDGE('',*,*,#5334,.F.);
#6872=ORIENTED_EDGE('',*,*,#5335,.T.);
#6873=ORIENTED_EDGE('',*,*,#5333,.T.);
#6874=ORIENTED_EDGE('',*,*,#5335,.F.);
#6875=ORIENTED_EDGE('',*,*,#5336,.F.);
#6876=ORIENTED_EDGE('',*,*,#5337,.T.);
#6877=ORIENTED_EDGE('',*,*,#5334,.T.);
#6878=ORIENTED_EDGE('',*,*,#5337,.F.);
#6879=ORIENTED_EDGE('',*,*,#5338,.F.);
#6880=ORIENTED_EDGE('',*,*,#5339,.T.);
#6881=ORIENTED_EDGE('',*,*,#5336,.T.);
#6882=ORIENTED_EDGE('',*,*,#5339,.F.);
#6883=ORIENTED_EDGE('',*,*,#5338,.T.);
#6884=ORIENTED_EDGE('',*,*,#5340,.T.);
#6885=ORIENTED_EDGE('',*,*,#5341,.T.);
#6886=ORIENTED_EDGE('',*,*,#5342,.T.);
#6887=ORIENTED_EDGE('',*,*,#5343,.F.);
#6888=ORIENTED_EDGE('',*,*,#5344,.T.);
#6889=ORIENTED_EDGE('',*,*,#5345,.T.);
#6890=ORIENTED_EDGE('',*,*,#5346,.T.);
#6891=ORIENTED_EDGE('',*,*,#5341,.F.);
#6892=ORIENTED_EDGE('',*,*,#5347,.T.);
#6893=ORIENTED_EDGE('',*,*,#5348,.T.);
#6894=ORIENTED_EDGE('',*,*,#5349,.T.);
#6895=ORIENTED_EDGE('',*,*,#5345,.F.);
#6896=ORIENTED_EDGE('',*,*,#5350,.T.);
#6897=ORIENTED_EDGE('',*,*,#5351,.T.);
#6898=ORIENTED_EDGE('',*,*,#5352,.T.);
#6899=ORIENTED_EDGE('',*,*,#5348,.F.);
#6900=ORIENTED_EDGE('',*,*,#5353,.T.);
#6901=ORIENTED_EDGE('',*,*,#5354,.T.);
#6902=ORIENTED_EDGE('',*,*,#5355,.T.);
#6903=ORIENTED_EDGE('',*,*,#5351,.F.);
#6904=ORIENTED_EDGE('',*,*,#5356,.T.);
#6905=ORIENTED_EDGE('',*,*,#5343,.T.);
#6906=ORIENTED_EDGE('',*,*,#5357,.T.);
#6907=ORIENTED_EDGE('',*,*,#5354,.F.);
#6908=ORIENTED_EDGE('',*,*,#5356,.F.);
#6909=ORIENTED_EDGE('',*,*,#5353,.F.);
#6910=ORIENTED_EDGE('',*,*,#5350,.F.);
#6911=ORIENTED_EDGE('',*,*,#5347,.F.);
#6912=ORIENTED_EDGE('',*,*,#5344,.F.);
#6913=ORIENTED_EDGE('',*,*,#5340,.F.);
#6914=ORIENTED_EDGE('',*,*,#5357,.F.);
#6915=ORIENTED_EDGE('',*,*,#5342,.F.);
#6916=ORIENTED_EDGE('',*,*,#5346,.F.);
#6917=ORIENTED_EDGE('',*,*,#5349,.F.);
#6918=ORIENTED_EDGE('',*,*,#5352,.F.);
#6919=ORIENTED_EDGE('',*,*,#5355,.F.);
#6920=ORIENTED_EDGE('',*,*,#5358,.F.);
#6921=ORIENTED_EDGE('',*,*,#5359,.F.);
#6922=ORIENTED_EDGE('',*,*,#5360,.F.);
#6923=ORIENTED_EDGE('',*,*,#5361,.T.);
#6924=ORIENTED_EDGE('',*,*,#5362,.F.);
#6925=ORIENTED_EDGE('',*,*,#5361,.F.);
#6926=ORIENTED_EDGE('',*,*,#5363,.F.);
#6927=ORIENTED_EDGE('',*,*,#5364,.F.);
#6928=ORIENTED_EDGE('',*,*,#5365,.F.);
#6929=ORIENTED_EDGE('',*,*,#5364,.T.);
#6930=ORIENTED_EDGE('',*,*,#5366,.T.);
#6931=ORIENTED_EDGE('',*,*,#5367,.F.);
#6932=ORIENTED_EDGE('',*,*,#5363,.T.);
#6933=ORIENTED_EDGE('',*,*,#5360,.T.);
#6934=ORIENTED_EDGE('',*,*,#5368,.F.);
#6935=ORIENTED_EDGE('',*,*,#5366,.F.);
#6936=ORIENTED_EDGE('',*,*,#5358,.T.);
#6937=ORIENTED_EDGE('',*,*,#5362,.T.);
#6938=ORIENTED_EDGE('',*,*,#5365,.T.);
#6939=ORIENTED_EDGE('',*,*,#5369,.F.);
#6940=ORIENTED_EDGE('',*,*,#5370,.T.);
#6941=ORIENTED_EDGE('',*,*,#5371,.T.);
#6942=ORIENTED_EDGE('',*,*,#5370,.F.);
#6943=ORIENTED_EDGE('',*,*,#5372,.F.);
#6944=ORIENTED_EDGE('',*,*,#5359,.T.);
#6945=ORIENTED_EDGE('',*,*,#5372,.T.);
#6946=ORIENTED_EDGE('',*,*,#5369,.T.);
#6947=ORIENTED_EDGE('',*,*,#5367,.T.);
#6948=ORIENTED_EDGE('',*,*,#5368,.T.);
#6949=ORIENTED_EDGE('',*,*,#5371,.F.);
#6950=ORIENTED_EDGE('',*,*,#5373,.F.);
#6951=ORIENTED_EDGE('',*,*,#5374,.T.);
#6952=ORIENTED_EDGE('',*,*,#5375,.F.);
#6953=ORIENTED_EDGE('',*,*,#5376,.F.);
#6954=ORIENTED_EDGE('',*,*,#5377,.T.);
#6955=ORIENTED_EDGE('',*,*,#5378,.F.);
#6956=ORIENTED_EDGE('',*,*,#5379,.F.);
#6957=ORIENTED_EDGE('',*,*,#5377,.F.);
#6958=ORIENTED_EDGE('',*,*,#5380,.F.);
#6959=ORIENTED_EDGE('',*,*,#5381,.F.);
#6960=ORIENTED_EDGE('',*,*,#5374,.F.);
#6961=ORIENTED_EDGE('',*,*,#5382,.F.);
#6962=ORIENTED_EDGE('',*,*,#5380,.T.);
#6963=ORIENTED_EDGE('',*,*,#5376,.T.);
#6964=ORIENTED_EDGE('',*,*,#5383,.F.);
#6965=ORIENTED_EDGE('',*,*,#5384,.T.);
#6966=ORIENTED_EDGE('',*,*,#5385,.T.);
#6967=ORIENTED_EDGE('',*,*,#5384,.F.);
#6968=ORIENTED_EDGE('',*,*,#5381,.T.);
#6969=ORIENTED_EDGE('',*,*,#5382,.T.);
#6970=ORIENTED_EDGE('',*,*,#5375,.T.);
#6971=ORIENTED_EDGE('',*,*,#5373,.T.);
#6972=ORIENTED_EDGE('',*,*,#5386,.F.);
#6973=ORIENTED_EDGE('',*,*,#5387,.T.);
#6974=ORIENTED_EDGE('',*,*,#5388,.T.);
#6975=ORIENTED_EDGE('',*,*,#5387,.F.);
#6976=ORIENTED_EDGE('',*,*,#5378,.T.);
#6977=ORIENTED_EDGE('',*,*,#5379,.T.);
#6978=ORIENTED_EDGE('',*,*,#5386,.T.);
#6979=ORIENTED_EDGE('',*,*,#5383,.T.);
#6980=ORIENTED_EDGE('',*,*,#5388,.F.);
#6981=ORIENTED_EDGE('',*,*,#5385,.F.);
#6982=ORIENTED_EDGE('',*,*,#5389,.F.);
#6983=ORIENTED_EDGE('',*,*,#5390,.T.);
#6984=ORIENTED_EDGE('',*,*,#5391,.F.);
#6985=ORIENTED_EDGE('',*,*,#5392,.F.);
#6986=ORIENTED_EDGE('',*,*,#5393,.T.);
#6987=ORIENTED_EDGE('',*,*,#5394,.F.);
#6988=ORIENTED_EDGE('',*,*,#5395,.F.);
#6989=ORIENTED_EDGE('',*,*,#5393,.F.);
#6990=ORIENTED_EDGE('',*,*,#5396,.F.);
#6991=ORIENTED_EDGE('',*,*,#5397,.F.);
#6992=ORIENTED_EDGE('',*,*,#5390,.F.);
#6993=ORIENTED_EDGE('',*,*,#5398,.F.);
#6994=ORIENTED_EDGE('',*,*,#5396,.T.);
#6995=ORIENTED_EDGE('',*,*,#5392,.T.);
#6996=ORIENTED_EDGE('',*,*,#5399,.F.);
#6997=ORIENTED_EDGE('',*,*,#5400,.T.);
#6998=ORIENTED_EDGE('',*,*,#5401,.T.);
#6999=ORIENTED_EDGE('',*,*,#5400,.F.);
#7000=ORIENTED_EDGE('',*,*,#5397,.T.);
#7001=ORIENTED_EDGE('',*,*,#5398,.T.);
#7002=ORIENTED_EDGE('',*,*,#5391,.T.);
#7003=ORIENTED_EDGE('',*,*,#5389,.T.);
#7004=ORIENTED_EDGE('',*,*,#5402,.F.);
#7005=ORIENTED_EDGE('',*,*,#5403,.T.);
#7006=ORIENTED_EDGE('',*,*,#5404,.T.);
#7007=ORIENTED_EDGE('',*,*,#5403,.F.);
#7008=ORIENTED_EDGE('',*,*,#5394,.T.);
#7009=ORIENTED_EDGE('',*,*,#5395,.T.);
#7010=ORIENTED_EDGE('',*,*,#5402,.T.);
#7011=ORIENTED_EDGE('',*,*,#5399,.T.);
#7012=ORIENTED_EDGE('',*,*,#5404,.F.);
#7013=ORIENTED_EDGE('',*,*,#5401,.F.);
#7014=ORIENTED_EDGE('',*,*,#5405,.F.);
#7015=ORIENTED_EDGE('',*,*,#5406,.T.);
#7016=ORIENTED_EDGE('',*,*,#5407,.T.);
#7017=ORIENTED_EDGE('',*,*,#5406,.F.);
#7018=ORIENTED_EDGE('',*,*,#5408,.F.);
#7019=ORIENTED_EDGE('',*,*,#5409,.T.);
#7020=ORIENTED_EDGE('',*,*,#5410,.T.);
#7021=ORIENTED_EDGE('',*,*,#5409,.F.);
#7022=ORIENTED_EDGE('',*,*,#5408,.T.);
#7023=ORIENTED_EDGE('',*,*,#5405,.T.);
#7024=ORIENTED_EDGE('',*,*,#5410,.F.);
#7025=ORIENTED_EDGE('',*,*,#5407,.F.);
#7026=ORIENTED_EDGE('',*,*,#5411,.F.);
#7027=ORIENTED_EDGE('',*,*,#5412,.T.);
#7028=ORIENTED_EDGE('',*,*,#5413,.F.);
#7029=ORIENTED_EDGE('',*,*,#5414,.F.);
#7030=ORIENTED_EDGE('',*,*,#5415,.T.);
#7031=ORIENTED_EDGE('',*,*,#5416,.F.);
#7032=ORIENTED_EDGE('',*,*,#5415,.F.);
#7033=ORIENTED_EDGE('',*,*,#5417,.F.);
#7034=ORIENTED_EDGE('',*,*,#5418,.F.);
#7035=ORIENTED_EDGE('',*,*,#5412,.F.);
#7036=ORIENTED_EDGE('',*,*,#5413,.T.);
#7037=ORIENTED_EDGE('',*,*,#5411,.T.);
#7038=ORIENTED_EDGE('',*,*,#5418,.T.);
#7039=ORIENTED_EDGE('',*,*,#5419,.T.);
#7040=ORIENTED_EDGE('',*,*,#5420,.T.);
#7041=ORIENTED_EDGE('',*,*,#5421,.T.);
#7042=ORIENTED_EDGE('',*,*,#5422,.T.);
#7043=ORIENTED_EDGE('',*,*,#5423,.T.);
#7044=ORIENTED_EDGE('',*,*,#5424,.T.);
#7045=ORIENTED_EDGE('',*,*,#5425,.T.);
#7046=ORIENTED_EDGE('',*,*,#5426,.T.);
#7047=ORIENTED_EDGE('',*,*,#5427,.T.);
#7048=ORIENTED_EDGE('',*,*,#5428,.T.);
#7049=ORIENTED_EDGE('',*,*,#5429,.T.);
#7050=ORIENTED_EDGE('',*,*,#5417,.T.);
#7051=ORIENTED_EDGE('',*,*,#5414,.T.);
#7052=ORIENTED_EDGE('',*,*,#5429,.F.);
#7053=ORIENTED_EDGE('',*,*,#5430,.F.);
#7054=ORIENTED_EDGE('',*,*,#5431,.F.);
#7055=ORIENTED_EDGE('',*,*,#5432,.F.);
#7056=ORIENTED_EDGE('',*,*,#5419,.F.);
#7057=ORIENTED_EDGE('',*,*,#5433,.T.);
#7058=ORIENTED_EDGE('',*,*,#5416,.T.);
#7059=ORIENTED_EDGE('',*,*,#5431,.T.);
#7060=ORIENTED_EDGE('',*,*,#5434,.F.);
#7061=ORIENTED_EDGE('',*,*,#5435,.F.);
#7062=ORIENTED_EDGE('',*,*,#5436,.T.);
#7063=ORIENTED_EDGE('',*,*,#5430,.T.);
#7064=ORIENTED_EDGE('',*,*,#5428,.F.);
#7065=ORIENTED_EDGE('',*,*,#5437,.F.);
#7066=ORIENTED_EDGE('',*,*,#5434,.T.);
#7067=ORIENTED_EDGE('',*,*,#5425,.F.);
#7068=ORIENTED_EDGE('',*,*,#5438,.T.);
#7069=ORIENTED_EDGE('',*,*,#5424,.F.);
#7070=ORIENTED_EDGE('',*,*,#5439,.F.);
#7071=ORIENTED_EDGE('',*,*,#5422,.F.);
#7072=ORIENTED_EDGE('',*,*,#5440,.F.);
#7073=ORIENTED_EDGE('',*,*,#5441,.F.);
#7074=ORIENTED_EDGE('',*,*,#5442,.F.);
#7075=ORIENTED_EDGE('',*,*,#5426,.F.);
#7076=ORIENTED_EDGE('',*,*,#5438,.F.);
#7077=ORIENTED_EDGE('',*,*,#5423,.F.);
#7078=ORIENTED_EDGE('',*,*,#5439,.T.);
#7079=ORIENTED_EDGE('',*,*,#5432,.T.);
#7080=ORIENTED_EDGE('',*,*,#5436,.F.);
#7081=ORIENTED_EDGE('',*,*,#5443,.F.);
#7082=ORIENTED_EDGE('',*,*,#5420,.F.);
#7083=ORIENTED_EDGE('',*,*,#5444,.F.);
#7084=ORIENTED_EDGE('',*,*,#5445,.F.);
#7085=ORIENTED_EDGE('',*,*,#5433,.F.);
#7086=ORIENTED_EDGE('',*,*,#5446,.T.);
#7087=ORIENTED_EDGE('',*,*,#5444,.T.);
#7088=ORIENTED_EDGE('',*,*,#5446,.F.);
#7089=ORIENTED_EDGE('',*,*,#5445,.T.);
#7090=ORIENTED_EDGE('',*,*,#5447,.T.);
#7091=ORIENTED_EDGE('',*,*,#5448,.T.);
#7092=ORIENTED_EDGE('',*,*,#5441,.T.);
#7093=ORIENTED_EDGE('',*,*,#5449,.T.);
#7094=ORIENTED_EDGE('',*,*,#5447,.F.);
#7095=ORIENTED_EDGE('',*,*,#5440,.T.);
#7096=ORIENTED_EDGE('',*,*,#5421,.F.);
#7097=ORIENTED_EDGE('',*,*,#5443,.T.);
#7098=ORIENTED_EDGE('',*,*,#5435,.T.);
#7099=ORIENTED_EDGE('',*,*,#5437,.T.);
#7100=ORIENTED_EDGE('',*,*,#5427,.F.);
#7101=ORIENTED_EDGE('',*,*,#5442,.T.);
#7102=ORIENTED_EDGE('',*,*,#5448,.F.);
#7103=ORIENTED_EDGE('',*,*,#5449,.F.);
#7104=ORIENTED_EDGE('',*,*,#5450,.F.);
#7105=ORIENTED_EDGE('',*,*,#5451,.T.);
#7106=ORIENTED_EDGE('',*,*,#5452,.F.);
#7107=ORIENTED_EDGE('',*,*,#5451,.F.);
#7108=ORIENTED_EDGE('',*,*,#5450,.T.);
#7109=ORIENTED_EDGE('',*,*,#5453,.F.);
#7110=ORIENTED_EDGE('',*,*,#5454,.T.);
#7111=ORIENTED_EDGE('',*,*,#5455,.F.);
#7112=ORIENTED_EDGE('',*,*,#5456,.T.);
#7113=ORIENTED_EDGE('',*,*,#5453,.T.);
#7114=ORIENTED_EDGE('',*,*,#5456,.F.);
#7115=ORIENTED_EDGE('',*,*,#5455,.T.);
#7116=ORIENTED_EDGE('',*,*,#5452,.T.);
#7117=ORIENTED_EDGE('',*,*,#5454,.F.);
#7118=ORIENTED_EDGE('',*,*,#5457,.T.);
#7119=ORIENTED_EDGE('',*,*,#5458,.T.);
#7120=ORIENTED_EDGE('',*,*,#5457,.F.);
#7121=ORIENTED_EDGE('',*,*,#5458,.F.);
#7122=ORIENTED_EDGE('',*,*,#5459,.F.);
#7123=ORIENTED_EDGE('',*,*,#5460,.T.);
#7124=ORIENTED_EDGE('',*,*,#5461,.T.);
#7125=ORIENTED_EDGE('',*,*,#5460,.F.);
#7126=ORIENTED_EDGE('',*,*,#5462,.F.);
#7127=ORIENTED_EDGE('',*,*,#5463,.T.);
#7128=ORIENTED_EDGE('',*,*,#5464,.T.);
#7129=ORIENTED_EDGE('',*,*,#5463,.F.);
#7130=ORIENTED_EDGE('',*,*,#5462,.T.);
#7131=ORIENTED_EDGE('',*,*,#5459,.T.);
#7132=ORIENTED_EDGE('',*,*,#5464,.F.);
#7133=ORIENTED_EDGE('',*,*,#5461,.F.);
#7134=ORIENTED_EDGE('',*,*,#5465,.F.);
#7135=ORIENTED_EDGE('',*,*,#5466,.T.);
#7136=ORIENTED_EDGE('',*,*,#5467,.T.);
#7137=ORIENTED_EDGE('',*,*,#5466,.F.);
#7138=ORIENTED_EDGE('',*,*,#5468,.F.);
#7139=ORIENTED_EDGE('',*,*,#5469,.T.);
#7140=ORIENTED_EDGE('',*,*,#5470,.T.);
#7141=ORIENTED_EDGE('',*,*,#5469,.F.);
#7142=ORIENTED_EDGE('',*,*,#5468,.T.);
#7143=ORIENTED_EDGE('',*,*,#5465,.T.);
#7144=ORIENTED_EDGE('',*,*,#5470,.F.);
#7145=ORIENTED_EDGE('',*,*,#5467,.F.);
#7146=ORIENTED_EDGE('',*,*,#5471,.F.);
#7147=ORIENTED_EDGE('',*,*,#5472,.T.);
#7148=ORIENTED_EDGE('',*,*,#5473,.T.);
#7149=ORIENTED_EDGE('',*,*,#5472,.F.);
#7150=ORIENTED_EDGE('',*,*,#5474,.F.);
#7151=ORIENTED_EDGE('',*,*,#5475,.T.);
#7152=ORIENTED_EDGE('',*,*,#5476,.T.);
#7153=ORIENTED_EDGE('',*,*,#5475,.F.);
#7154=ORIENTED_EDGE('',*,*,#5474,.T.);
#7155=ORIENTED_EDGE('',*,*,#5471,.T.);
#7156=ORIENTED_EDGE('',*,*,#5476,.F.);
#7157=ORIENTED_EDGE('',*,*,#5473,.F.);
#7158=ORIENTED_EDGE('',*,*,#5477,.F.);
#7159=ORIENTED_EDGE('',*,*,#5478,.F.);
#7160=ORIENTED_EDGE('',*,*,#5479,.F.);
#7161=ORIENTED_EDGE('',*,*,#5480,.F.);
#7162=ORIENTED_EDGE('',*,*,#5481,.F.);
#7163=ORIENTED_EDGE('',*,*,#5482,.F.);
#7164=ORIENTED_EDGE('',*,*,#5483,.F.);
#7165=ORIENTED_EDGE('',*,*,#5484,.F.);
#7166=ORIENTED_EDGE('',*,*,#5481,.T.);
#7167=ORIENTED_EDGE('',*,*,#5485,.T.);
#7168=ORIENTED_EDGE('',*,*,#5486,.T.);
#7169=ORIENTED_EDGE('',*,*,#5487,.T.);
#7170=ORIENTED_EDGE('',*,*,#5480,.T.);
#7171=ORIENTED_EDGE('',*,*,#5488,.F.);
#7172=ORIENTED_EDGE('',*,*,#5489,.T.);
#7173=ORIENTED_EDGE('',*,*,#5485,.F.);
#7174=ORIENTED_EDGE('',*,*,#5479,.T.);
#7175=ORIENTED_EDGE('',*,*,#5490,.T.);
#7176=ORIENTED_EDGE('',*,*,#5491,.T.);
#7177=ORIENTED_EDGE('',*,*,#5488,.T.);
#7178=ORIENTED_EDGE('',*,*,#5478,.T.);
#7179=ORIENTED_EDGE('',*,*,#5492,.F.);
#7180=ORIENTED_EDGE('',*,*,#5493,.T.);
#7181=ORIENTED_EDGE('',*,*,#5490,.F.);
#7182=ORIENTED_EDGE('',*,*,#5494,.F.);
#7183=ORIENTED_EDGE('',*,*,#5495,.F.);
#7184=ORIENTED_EDGE('',*,*,#5486,.F.);
#7185=ORIENTED_EDGE('',*,*,#5489,.F.);
#7186=ORIENTED_EDGE('',*,*,#5491,.F.);
#7187=ORIENTED_EDGE('',*,*,#5493,.F.);
#7188=ORIENTED_EDGE('',*,*,#5496,.F.);
#7189=ORIENTED_EDGE('',*,*,#5497,.F.);
#7190=ORIENTED_EDGE('',*,*,#5482,.T.);
#7191=ORIENTED_EDGE('',*,*,#5487,.F.);
#7192=ORIENTED_EDGE('',*,*,#5495,.T.);
#7193=ORIENTED_EDGE('',*,*,#5498,.F.);
#7194=ORIENTED_EDGE('',*,*,#5477,.T.);
#7195=ORIENTED_EDGE('',*,*,#5499,.T.);
#7196=ORIENTED_EDGE('',*,*,#5496,.T.);
#7197=ORIENTED_EDGE('',*,*,#5492,.T.);
#7198=ORIENTED_EDGE('',*,*,#5483,.T.);
#7199=ORIENTED_EDGE('',*,*,#5498,.T.);
#7200=ORIENTED_EDGE('',*,*,#5494,.T.);
#7201=ORIENTED_EDGE('',*,*,#5500,.T.);
#7202=ORIENTED_EDGE('',*,*,#5484,.T.);
#7203=ORIENTED_EDGE('',*,*,#5500,.F.);
#7204=ORIENTED_EDGE('',*,*,#5497,.T.);
#7205=ORIENTED_EDGE('',*,*,#5499,.F.);
#7206=ORIENTED_EDGE('',*,*,#5501,.F.);
#7207=ORIENTED_EDGE('',*,*,#5502,.T.);
#7208=ORIENTED_EDGE('',*,*,#5503,.T.);
#7209=ORIENTED_EDGE('',*,*,#5504,.F.);
#7210=ORIENTED_EDGE('',*,*,#5505,.F.);
#7211=ORIENTED_EDGE('',*,*,#5506,.T.);
#7212=ORIENTED_EDGE('',*,*,#5507,.T.);
#7213=ORIENTED_EDGE('',*,*,#5502,.F.);
#7214=ORIENTED_EDGE('',*,*,#5508,.F.);
#7215=ORIENTED_EDGE('',*,*,#5509,.T.);
#7216=ORIENTED_EDGE('',*,*,#5510,.T.);
#7217=ORIENTED_EDGE('',*,*,#5506,.F.);
#7218=ORIENTED_EDGE('',*,*,#5511,.F.);
#7219=ORIENTED_EDGE('',*,*,#5512,.T.);
#7220=ORIENTED_EDGE('',*,*,#5513,.T.);
#7221=ORIENTED_EDGE('',*,*,#5509,.F.);
#7222=ORIENTED_EDGE('',*,*,#5514,.F.);
#7223=ORIENTED_EDGE('',*,*,#5515,.T.);
#7224=ORIENTED_EDGE('',*,*,#5516,.T.);
#7225=ORIENTED_EDGE('',*,*,#5512,.F.);
#7226=ORIENTED_EDGE('',*,*,#5517,.F.);
#7227=ORIENTED_EDGE('',*,*,#5504,.T.);
#7228=ORIENTED_EDGE('',*,*,#5518,.T.);
#7229=ORIENTED_EDGE('',*,*,#5515,.F.);
#7230=ORIENTED_EDGE('',*,*,#5518,.F.);
#7231=ORIENTED_EDGE('',*,*,#5503,.F.);
#7232=ORIENTED_EDGE('',*,*,#5507,.F.);
#7233=ORIENTED_EDGE('',*,*,#5510,.F.);
#7234=ORIENTED_EDGE('',*,*,#5513,.F.);
#7235=ORIENTED_EDGE('',*,*,#5516,.F.);
#7236=ORIENTED_EDGE('',*,*,#5519,.F.);
#7237=ORIENTED_EDGE('',*,*,#5501,.T.);
#7238=ORIENTED_EDGE('',*,*,#5517,.T.);
#7239=ORIENTED_EDGE('',*,*,#5514,.T.);
#7240=ORIENTED_EDGE('',*,*,#5511,.T.);
#7241=ORIENTED_EDGE('',*,*,#5508,.T.);
#7242=ORIENTED_EDGE('',*,*,#5505,.T.);
#7243=ORIENTED_EDGE('',*,*,#5520,.F.);
#7244=ORIENTED_EDGE('',*,*,#5521,.T.);
#7245=ORIENTED_EDGE('',*,*,#5519,.T.);
#7246=ORIENTED_EDGE('',*,*,#5521,.F.);
#7247=ORIENTED_EDGE('',*,*,#5522,.F.);
#7248=ORIENTED_EDGE('',*,*,#5523,.T.);
#7249=ORIENTED_EDGE('',*,*,#5520,.T.);
#7250=ORIENTED_EDGE('',*,*,#5523,.F.);
#7251=ORIENTED_EDGE('',*,*,#5524,.F.);
#7252=ORIENTED_EDGE('',*,*,#5525,.T.);
#7253=ORIENTED_EDGE('',*,*,#5522,.T.);
#7254=ORIENTED_EDGE('',*,*,#5525,.F.);
#7255=ORIENTED_EDGE('',*,*,#5524,.T.);
#7256=ORIENTED_EDGE('',*,*,#5526,.F.);
#7257=ORIENTED_EDGE('',*,*,#5527,.T.);
#7258=ORIENTED_EDGE('',*,*,#5528,.F.);
#7259=ORIENTED_EDGE('',*,*,#5527,.F.);
#7260=ORIENTED_EDGE('',*,*,#5529,.F.);
#7261=ORIENTED_EDGE('',*,*,#5530,.T.);
#7262=ORIENTED_EDGE('',*,*,#5531,.F.);
#7263=ORIENTED_EDGE('',*,*,#5530,.F.);
#7264=ORIENTED_EDGE('',*,*,#5532,.F.);
#7265=ORIENTED_EDGE('',*,*,#5533,.T.);
#7266=ORIENTED_EDGE('',*,*,#5534,.F.);
#7267=ORIENTED_EDGE('',*,*,#5535,.F.);
#7268=ORIENTED_EDGE('',*,*,#5535,.T.);
#7269=ORIENTED_EDGE('',*,*,#5536,.T.);
#7270=ORIENTED_EDGE('',*,*,#5537,.T.);
#7271=ORIENTED_EDGE('',*,*,#5538,.T.);
#7272=ORIENTED_EDGE('',*,*,#5528,.T.);
#7273=ORIENTED_EDGE('',*,*,#5531,.T.);
#7274=ORIENTED_EDGE('',*,*,#5534,.T.);
#7275=ORIENTED_EDGE('',*,*,#5539,.F.);
#7276=ORIENTED_EDGE('',*,*,#5540,.T.);
#7277=ORIENTED_EDGE('',*,*,#5536,.F.);
#7278=ORIENTED_EDGE('',*,*,#5541,.F.);
#7279=ORIENTED_EDGE('',*,*,#5537,.F.);
#7280=ORIENTED_EDGE('',*,*,#5540,.F.);
#7281=ORIENTED_EDGE('',*,*,#5542,.T.);
#7282=ORIENTED_EDGE('',*,*,#5532,.T.);
#7283=ORIENTED_EDGE('',*,*,#5538,.F.);
#7284=ORIENTED_EDGE('',*,*,#5541,.T.);
#7285=ORIENTED_EDGE('',*,*,#5543,.F.);
#7286=ORIENTED_EDGE('',*,*,#5543,.T.);
#7287=ORIENTED_EDGE('',*,*,#5542,.F.);
#7288=ORIENTED_EDGE('',*,*,#5539,.T.);
#7289=ORIENTED_EDGE('',*,*,#5533,.F.);
#7290=ORIENTED_EDGE('',*,*,#5526,.T.);
#7291=ORIENTED_EDGE('',*,*,#5529,.T.);
#7292=ORIENTED_EDGE('',*,*,#5544,.F.);
#7293=ORIENTED_EDGE('',*,*,#5545,.T.);
#7294=ORIENTED_EDGE('',*,*,#5546,.T.);
#7295=ORIENTED_EDGE('',*,*,#5545,.F.);
#7296=ORIENTED_EDGE('',*,*,#5547,.F.);
#7297=ORIENTED_EDGE('',*,*,#5548,.T.);
#7298=ORIENTED_EDGE('',*,*,#5549,.T.);
#7299=ORIENTED_EDGE('',*,*,#5548,.F.);
#7300=ORIENTED_EDGE('',*,*,#5547,.T.);
#7301=ORIENTED_EDGE('',*,*,#5544,.T.);
#7302=ORIENTED_EDGE('',*,*,#5549,.F.);
#7303=ORIENTED_EDGE('',*,*,#5546,.F.);
#7304=ORIENTED_EDGE('',*,*,#5550,.F.);
#7305=ORIENTED_EDGE('',*,*,#5551,.T.);
#7306=ORIENTED_EDGE('',*,*,#5552,.T.);
#7307=ORIENTED_EDGE('',*,*,#5551,.F.);
#7308=ORIENTED_EDGE('',*,*,#5553,.F.);
#7309=ORIENTED_EDGE('',*,*,#5554,.T.);
#7310=ORIENTED_EDGE('',*,*,#5555,.T.);
#7311=ORIENTED_EDGE('',*,*,#5554,.F.);
#7312=ORIENTED_EDGE('',*,*,#5553,.T.);
#7313=ORIENTED_EDGE('',*,*,#5550,.T.);
#7314=ORIENTED_EDGE('',*,*,#5555,.F.);
#7315=ORIENTED_EDGE('',*,*,#5552,.F.);
#7316=ORIENTED_EDGE('',*,*,#5556,.F.);
#7317=ORIENTED_EDGE('',*,*,#5557,.T.);
#7318=ORIENTED_EDGE('',*,*,#5558,.T.);
#7319=ORIENTED_EDGE('',*,*,#5557,.F.);
#7320=ORIENTED_EDGE('',*,*,#5559,.F.);
#7321=ORIENTED_EDGE('',*,*,#5560,.T.);
#7322=ORIENTED_EDGE('',*,*,#5561,.T.);
#7323=ORIENTED_EDGE('',*,*,#5560,.F.);
#7324=ORIENTED_EDGE('',*,*,#5559,.T.);
#7325=ORIENTED_EDGE('',*,*,#5556,.T.);
#7326=ORIENTED_EDGE('',*,*,#5561,.F.);
#7327=ORIENTED_EDGE('',*,*,#5558,.F.);
#7328=ORIENTED_EDGE('',*,*,#5562,.F.);
#7329=ORIENTED_EDGE('',*,*,#5563,.T.);
#7330=ORIENTED_EDGE('',*,*,#5564,.T.);
#7331=ORIENTED_EDGE('',*,*,#5563,.F.);
#7332=ORIENTED_EDGE('',*,*,#5565,.F.);
#7333=ORIENTED_EDGE('',*,*,#5566,.T.);
#7334=ORIENTED_EDGE('',*,*,#5567,.T.);
#7335=ORIENTED_EDGE('',*,*,#5566,.F.);
#7336=ORIENTED_EDGE('',*,*,#5565,.T.);
#7337=ORIENTED_EDGE('',*,*,#5562,.T.);
#7338=ORIENTED_EDGE('',*,*,#5567,.F.);
#7339=ORIENTED_EDGE('',*,*,#5564,.F.);
#7340=ORIENTED_EDGE('',*,*,#5568,.F.);
#7341=ORIENTED_EDGE('',*,*,#5569,.F.);
#7342=ORIENTED_EDGE('',*,*,#5570,.T.);
#7343=ORIENTED_EDGE('',*,*,#5571,.F.);
#7344=ORIENTED_EDGE('',*,*,#5572,.F.);
#7345=ORIENTED_EDGE('',*,*,#5570,.F.);
#7346=ORIENTED_EDGE('',*,*,#5571,.T.);
#7347=ORIENTED_EDGE('',*,*,#5572,.T.);
#7348=ORIENTED_EDGE('',*,*,#5573,.T.);
#7349=ORIENTED_EDGE('',*,*,#5574,.T.);
#7350=ORIENTED_EDGE('',*,*,#5573,.F.);
#7351=ORIENTED_EDGE('',*,*,#5575,.T.);
#7352=ORIENTED_EDGE('',*,*,#5576,.T.);
#7353=ORIENTED_EDGE('',*,*,#5577,.F.);
#7354=ORIENTED_EDGE('',*,*,#5576,.F.);
#7355=ORIENTED_EDGE('',*,*,#5577,.T.);
#7356=ORIENTED_EDGE('',*,*,#5578,.T.);
#7357=ORIENTED_EDGE('',*,*,#5579,.F.);
#7358=ORIENTED_EDGE('',*,*,#5578,.F.);
#7359=ORIENTED_EDGE('',*,*,#5574,.F.);
#7360=ORIENTED_EDGE('',*,*,#5579,.T.);
#7361=ORIENTED_EDGE('',*,*,#5580,.F.);
#7362=ORIENTED_EDGE('',*,*,#5581,.T.);
#7363=ORIENTED_EDGE('',*,*,#5568,.T.);
#7364=ORIENTED_EDGE('',*,*,#5569,.T.);
#7365=ORIENTED_EDGE('',*,*,#5581,.F.);
#7366=ORIENTED_EDGE('',*,*,#5580,.T.);
#7367=ORIENTED_EDGE('',*,*,#5582,.F.);
#7368=ORIENTED_EDGE('',*,*,#5582,.T.);
#7369=ORIENTED_EDGE('',*,*,#5583,.T.);
#7370=ORIENTED_EDGE('',*,*,#5575,.F.);
#7371=ORIENTED_EDGE('',*,*,#5583,.F.);
#7372=ORIENTED_EDGE('',*,*,#5584,.F.);
#7373=ORIENTED_EDGE('',*,*,#5585,.F.);
#7374=ORIENTED_EDGE('',*,*,#5586,.T.);
#7375=ORIENTED_EDGE('',*,*,#5587,.F.);
#7376=ORIENTED_EDGE('',*,*,#5588,.F.);
#7377=ORIENTED_EDGE('',*,*,#5586,.F.);
#7378=ORIENTED_EDGE('',*,*,#5589,.T.);
#7379=ORIENTED_EDGE('',*,*,#5590,.T.);
#7380=ORIENTED_EDGE('',*,*,#5587,.T.);
#7381=ORIENTED_EDGE('',*,*,#5588,.T.);
#7382=ORIENTED_EDGE('',*,*,#5590,.F.);
#7383=ORIENTED_EDGE('',*,*,#5591,.F.);
#7384=ORIENTED_EDGE('',*,*,#5592,.T.);
#7385=ORIENTED_EDGE('',*,*,#5593,.F.);
#7386=ORIENTED_EDGE('',*,*,#5594,.T.);
#7387=ORIENTED_EDGE('',*,*,#5591,.T.);
#7388=ORIENTED_EDGE('',*,*,#5594,.F.);
#7389=ORIENTED_EDGE('',*,*,#5595,.F.);
#7390=ORIENTED_EDGE('',*,*,#5596,.T.);
#7391=ORIENTED_EDGE('',*,*,#5593,.T.);
#7392=ORIENTED_EDGE('',*,*,#5596,.F.);
#7393=ORIENTED_EDGE('',*,*,#5597,.F.);
#7394=ORIENTED_EDGE('',*,*,#5598,.T.);
#7395=ORIENTED_EDGE('',*,*,#5595,.T.);
#7396=ORIENTED_EDGE('',*,*,#5598,.F.);
#7397=ORIENTED_EDGE('',*,*,#5597,.T.);
#7398=ORIENTED_EDGE('',*,*,#5589,.F.);
#7399=ORIENTED_EDGE('',*,*,#5584,.T.);
#7400=ORIENTED_EDGE('',*,*,#5585,.T.);
#7401=ORIENTED_EDGE('',*,*,#5599,.T.);
#7402=ORIENTED_EDGE('',*,*,#5592,.F.);
#7403=ORIENTED_EDGE('',*,*,#5599,.F.);
#7404=ORIENTED_EDGE('',*,*,#5600,.T.);
#7405=ORIENTED_EDGE('',*,*,#5600,.F.);
#7406=ORIENTED_EDGE('',*,*,#5601,.T.);
#7407=ORIENTED_EDGE('',*,*,#5601,.F.);
#7408=ORIENTED_EDGE('',*,*,#5602,.T.);
#7409=ORIENTED_EDGE('',*,*,#5602,.F.);
#7410=ORIENTED_EDGE('',*,*,#5603,.T.);
#7411=ORIENTED_EDGE('',*,*,#5603,.F.);
#7412=ORIENTED_EDGE('',*,*,#5604,.T.);
#7413=ORIENTED_EDGE('',*,*,#5604,.F.);
#7414=ORIENTED_EDGE('',*,*,#5605,.T.);
#7415=ORIENTED_EDGE('',*,*,#5605,.F.);
#7416=ORIENTED_EDGE('',*,*,#5606,.T.);
#7417=ORIENTED_EDGE('',*,*,#5606,.F.);
#7418=ORIENTED_EDGE('',*,*,#5607,.T.);
#7419=ORIENTED_EDGE('',*,*,#5607,.F.);
#7420=ORIENTED_EDGE('',*,*,#5608,.F.);
#7421=ORIENTED_EDGE('',*,*,#5609,.F.);
#7422=ORIENTED_EDGE('',*,*,#5610,.F.);
#7423=ORIENTED_EDGE('',*,*,#5611,.F.);
#7424=ORIENTED_EDGE('',*,*,#5610,.T.);
#7425=ORIENTED_EDGE('',*,*,#5612,.F.);
#7426=ORIENTED_EDGE('',*,*,#5613,.T.);
#7427=ORIENTED_EDGE('',*,*,#5614,.F.);
#7428=ORIENTED_EDGE('',*,*,#5615,.T.);
#7429=ORIENTED_EDGE('',*,*,#5616,.F.);
#7430=ORIENTED_EDGE('',*,*,#5617,.T.);
#7431=ORIENTED_EDGE('',*,*,#5618,.T.);
#7432=ORIENTED_EDGE('',*,*,#5619,.F.);
#7433=ORIENTED_EDGE('',*,*,#5618,.F.);
#7434=ORIENTED_EDGE('',*,*,#5620,.T.);
#7435=ORIENTED_EDGE('',*,*,#5621,.F.);
#7436=ORIENTED_EDGE('',*,*,#5622,.T.);
#7437=ORIENTED_EDGE('',*,*,#5623,.F.);
#7438=ORIENTED_EDGE('',*,*,#5624,.T.);
#7439=ORIENTED_EDGE('',*,*,#5625,.F.);
#7440=ORIENTED_EDGE('',*,*,#5626,.T.);
#7441=ORIENTED_EDGE('',*,*,#5627,.F.);
#7442=ORIENTED_EDGE('',*,*,#5628,.T.);
#7443=ORIENTED_EDGE('',*,*,#5629,.F.);
#7444=ORIENTED_EDGE('',*,*,#5609,.T.);
#7445=ORIENTED_EDGE('',*,*,#5630,.T.);
#7446=ORIENTED_EDGE('',*,*,#5631,.T.);
#7447=ORIENTED_EDGE('',*,*,#5612,.T.);
#7448=ORIENTED_EDGE('',*,*,#5632,.F.);
#7449=ORIENTED_EDGE('',*,*,#5633,.F.);
#7450=ORIENTED_EDGE('',*,*,#5613,.F.);
#7451=ORIENTED_EDGE('',*,*,#5631,.F.);
#7452=ORIENTED_EDGE('',*,*,#5633,.T.);
#7453=ORIENTED_EDGE('',*,*,#5634,.T.);
#7454=ORIENTED_EDGE('',*,*,#5635,.T.);
#7455=ORIENTED_EDGE('',*,*,#5614,.T.);
#7456=ORIENTED_EDGE('',*,*,#5636,.F.);
#7457=ORIENTED_EDGE('',*,*,#5637,.F.);
#7458=ORIENTED_EDGE('',*,*,#5615,.F.);
#7459=ORIENTED_EDGE('',*,*,#5635,.F.);
#7460=ORIENTED_EDGE('',*,*,#5637,.T.);
#7461=ORIENTED_EDGE('',*,*,#5638,.T.);
#7462=ORIENTED_EDGE('',*,*,#5639,.T.);
#7463=ORIENTED_EDGE('',*,*,#5616,.T.);
#7464=ORIENTED_EDGE('',*,*,#5640,.F.);
#7465=ORIENTED_EDGE('',*,*,#5641,.F.);
#7466=ORIENTED_EDGE('',*,*,#5620,.F.);
#7467=ORIENTED_EDGE('',*,*,#5617,.F.);
#7468=ORIENTED_EDGE('',*,*,#5639,.F.);
#7469=ORIENTED_EDGE('',*,*,#5642,.F.);
#7470=ORIENTED_EDGE('',*,*,#5641,.T.);
#7471=ORIENTED_EDGE('',*,*,#5643,.T.);
#7472=ORIENTED_EDGE('',*,*,#5644,.T.);
#7473=ORIENTED_EDGE('',*,*,#5621,.T.);
#7474=ORIENTED_EDGE('',*,*,#5645,.F.);
#7475=ORIENTED_EDGE('',*,*,#5646,.F.);
#7476=ORIENTED_EDGE('',*,*,#5622,.F.);
#7477=ORIENTED_EDGE('',*,*,#5644,.F.);
#7478=ORIENTED_EDGE('',*,*,#5646,.T.);
#7479=ORIENTED_EDGE('',*,*,#5647,.T.);
#7480=ORIENTED_EDGE('',*,*,#5648,.T.);
#7481=ORIENTED_EDGE('',*,*,#5623,.T.);
#7482=ORIENTED_EDGE('',*,*,#5649,.F.);
#7483=ORIENTED_EDGE('',*,*,#5650,.F.);
#7484=ORIENTED_EDGE('',*,*,#5624,.F.);
#7485=ORIENTED_EDGE('',*,*,#5648,.F.);
#7486=ORIENTED_EDGE('',*,*,#5650,.T.);
#7487=ORIENTED_EDGE('',*,*,#5651,.T.);
#7488=ORIENTED_EDGE('',*,*,#5652,.T.);
#7489=ORIENTED_EDGE('',*,*,#5625,.T.);
#7490=ORIENTED_EDGE('',*,*,#5626,.F.);
#7491=ORIENTED_EDGE('',*,*,#5652,.F.);
#7492=ORIENTED_EDGE('',*,*,#5653,.F.);
#7493=ORIENTED_EDGE('',*,*,#5654,.F.);
#7494=ORIENTED_EDGE('',*,*,#5655,.F.);
#7495=ORIENTED_EDGE('',*,*,#5656,.T.);
#7496=ORIENTED_EDGE('',*,*,#5642,.T.);
#7497=ORIENTED_EDGE('',*,*,#5638,.F.);
#7498=ORIENTED_EDGE('',*,*,#5636,.T.);
#7499=ORIENTED_EDGE('',*,*,#5634,.F.);
#7500=ORIENTED_EDGE('',*,*,#5632,.T.);
#7501=ORIENTED_EDGE('',*,*,#5630,.F.);
#7502=ORIENTED_EDGE('',*,*,#5608,.T.);
#7503=ORIENTED_EDGE('',*,*,#5657,.F.);
#7504=ORIENTED_EDGE('',*,*,#5658,.T.);
#7505=ORIENTED_EDGE('',*,*,#5659,.F.);
#7506=ORIENTED_EDGE('',*,*,#5653,.T.);
#7507=ORIENTED_EDGE('',*,*,#5651,.F.);
#7508=ORIENTED_EDGE('',*,*,#5649,.T.);
#7509=ORIENTED_EDGE('',*,*,#5647,.F.);
#7510=ORIENTED_EDGE('',*,*,#5645,.T.);
#7511=ORIENTED_EDGE('',*,*,#5643,.F.);
#7512=ORIENTED_EDGE('',*,*,#5640,.T.);
#7513=ORIENTED_EDGE('',*,*,#5656,.F.);
#7514=ORIENTED_EDGE('',*,*,#5611,.T.);
#7515=ORIENTED_EDGE('',*,*,#5629,.T.);
#7516=ORIENTED_EDGE('',*,*,#5660,.T.);
#7517=ORIENTED_EDGE('',*,*,#5657,.T.);
#7518=ORIENTED_EDGE('',*,*,#5628,.F.);
#7519=ORIENTED_EDGE('',*,*,#5661,.F.);
#7520=ORIENTED_EDGE('',*,*,#5658,.F.);
#7521=ORIENTED_EDGE('',*,*,#5660,.F.);
#7522=ORIENTED_EDGE('',*,*,#5619,.T.);
#7523=ORIENTED_EDGE('',*,*,#5655,.T.);
#7524=ORIENTED_EDGE('',*,*,#5654,.T.);
#7525=ORIENTED_EDGE('',*,*,#5659,.T.);
#7526=ORIENTED_EDGE('',*,*,#5661,.T.);
#7527=ORIENTED_EDGE('',*,*,#5627,.T.);
#7528=ORIENTED_EDGE('',*,*,#5662,.F.);
#7529=ORIENTED_EDGE('',*,*,#5663,.T.);
#7530=ORIENTED_EDGE('',*,*,#5664,.F.);
#7531=ORIENTED_EDGE('',*,*,#5665,.T.);
#7532=ORIENTED_EDGE('',*,*,#5662,.T.);
#7533=ORIENTED_EDGE('',*,*,#5665,.F.);
#7534=ORIENTED_EDGE('',*,*,#5664,.T.);
#7535=ORIENTED_EDGE('',*,*,#5666,.F.);
#7536=ORIENTED_EDGE('',*,*,#5666,.T.);
#7537=ORIENTED_EDGE('',*,*,#5667,.T.);
#7538=ORIENTED_EDGE('',*,*,#5663,.F.);
#7539=ORIENTED_EDGE('',*,*,#5667,.F.);
#7540=ORIENTED_EDGE('',*,*,#5668,.F.);
#7541=ORIENTED_EDGE('',*,*,#5669,.T.);
#7542=ORIENTED_EDGE('',*,*,#5670,.F.);
#7543=ORIENTED_EDGE('',*,*,#5671,.T.);
#7544=ORIENTED_EDGE('',*,*,#5668,.T.);
#7545=ORIENTED_EDGE('',*,*,#5671,.F.);
#7546=ORIENTED_EDGE('',*,*,#5670,.T.);
#7547=ORIENTED_EDGE('',*,*,#5672,.F.);
#7548=ORIENTED_EDGE('',*,*,#5672,.T.);
#7549=ORIENTED_EDGE('',*,*,#5673,.T.);
#7550=ORIENTED_EDGE('',*,*,#5669,.F.);
#7551=ORIENTED_EDGE('',*,*,#5673,.F.);
#7552=ORIENTED_EDGE('',*,*,#5674,.F.);
#7553=ORIENTED_EDGE('',*,*,#5675,.T.);
#7554=ORIENTED_EDGE('',*,*,#5676,.F.);
#7555=ORIENTED_EDGE('',*,*,#5675,.F.);
#7556=ORIENTED_EDGE('',*,*,#5674,.T.);
#7557=ORIENTED_EDGE('',*,*,#5677,.F.);
#7558=ORIENTED_EDGE('',*,*,#5678,.T.);
#7559=ORIENTED_EDGE('',*,*,#5679,.F.);
#7560=ORIENTED_EDGE('',*,*,#5678,.F.);
#7561=ORIENTED_EDGE('',*,*,#5677,.T.);
#7562=ORIENTED_EDGE('',*,*,#5680,.F.);
#7563=ORIENTED_EDGE('',*,*,#5681,.T.);
#7564=ORIENTED_EDGE('',*,*,#5682,.F.);
#7565=ORIENTED_EDGE('',*,*,#5683,.F.);
#7566=ORIENTED_EDGE('',*,*,#5684,.F.);
#7567=ORIENTED_EDGE('',*,*,#5685,.F.);
#7568=ORIENTED_EDGE('',*,*,#5686,.F.);
#7569=ORIENTED_EDGE('',*,*,#5687,.F.);
#7570=ORIENTED_EDGE('',*,*,#5688,.F.);
#7571=ORIENTED_EDGE('',*,*,#5687,.T.);
#7572=ORIENTED_EDGE('',*,*,#5689,.F.);
#7573=ORIENTED_EDGE('',*,*,#5681,.F.);
#7574=ORIENTED_EDGE('',*,*,#5676,.T.);
#7575=ORIENTED_EDGE('',*,*,#5679,.T.);
#7576=ORIENTED_EDGE('',*,*,#5689,.T.);
#7577=ORIENTED_EDGE('',*,*,#5686,.T.);
#7578=ORIENTED_EDGE('',*,*,#5690,.F.);
#7579=ORIENTED_EDGE('',*,*,#5682,.T.);
#7580=ORIENTED_EDGE('',*,*,#5691,.F.);
#7581=ORIENTED_EDGE('',*,*,#5692,.T.);
#7582=ORIENTED_EDGE('',*,*,#5693,.F.);
#7583=ORIENTED_EDGE('',*,*,#5692,.F.);
#7584=ORIENTED_EDGE('',*,*,#5694,.F.);
#7585=ORIENTED_EDGE('',*,*,#5695,.T.);
#7586=ORIENTED_EDGE('',*,*,#5696,.T.);
#7587=ORIENTED_EDGE('',*,*,#5697,.T.);
#7588=ORIENTED_EDGE('',*,*,#5691,.T.);
#7589=ORIENTED_EDGE('',*,*,#5698,.F.);
#7590=ORIENTED_EDGE('',*,*,#5699,.F.);
#7591=ORIENTED_EDGE('',*,*,#5700,.F.);
#7592=ORIENTED_EDGE('',*,*,#5695,.F.);
#7593=ORIENTED_EDGE('',*,*,#5701,.F.);
#7594=ORIENTED_EDGE('',*,*,#5697,.F.);
#7595=ORIENTED_EDGE('',*,*,#5702,.T.);
#7596=ORIENTED_EDGE('',*,*,#5703,.F.);
#7597=ORIENTED_EDGE('',*,*,#5696,.F.);
#7598=ORIENTED_EDGE('',*,*,#5700,.T.);
#7599=ORIENTED_EDGE('',*,*,#5704,.F.);
#7600=ORIENTED_EDGE('',*,*,#5702,.F.);
#7601=ORIENTED_EDGE('',*,*,#5705,.F.);
#7602=ORIENTED_EDGE('',*,*,#5703,.T.);
#7603=ORIENTED_EDGE('',*,*,#5704,.T.);
#7604=ORIENTED_EDGE('',*,*,#5699,.T.);
#7605=ORIENTED_EDGE('',*,*,#5693,.T.);
#7606=ORIENTED_EDGE('',*,*,#5706,.F.);
#7607=ORIENTED_EDGE('',*,*,#5707,.T.);
#7608=ORIENTED_EDGE('',*,*,#5708,.F.);
#7609=ORIENTED_EDGE('',*,*,#5707,.F.);
#7610=ORIENTED_EDGE('',*,*,#5709,.F.);
#7611=ORIENTED_EDGE('',*,*,#5710,.T.);
#7612=ORIENTED_EDGE('',*,*,#5711,.F.);
#7613=ORIENTED_EDGE('',*,*,#5710,.F.);
#7614=ORIENTED_EDGE('',*,*,#5712,.F.);
#7615=ORIENTED_EDGE('',*,*,#5713,.T.);
#7616=ORIENTED_EDGE('',*,*,#5714,.F.);
#7617=ORIENTED_EDGE('',*,*,#5713,.F.);
#7618=ORIENTED_EDGE('',*,*,#5715,.F.);
#7619=ORIENTED_EDGE('',*,*,#5716,.T.);
#7620=ORIENTED_EDGE('',*,*,#5717,.F.);
#7621=ORIENTED_EDGE('',*,*,#5716,.F.);
#7622=ORIENTED_EDGE('',*,*,#5718,.T.);
#7623=ORIENTED_EDGE('',*,*,#5719,.T.);
#7624=ORIENTED_EDGE('',*,*,#5720,.F.);
#7625=ORIENTED_EDGE('',*,*,#5721,.F.);
#7626=ORIENTED_EDGE('',*,*,#5722,.T.);
#7627=ORIENTED_EDGE('',*,*,#5721,.T.);
#7628=ORIENTED_EDGE('',*,*,#5723,.F.);
#7629=ORIENTED_EDGE('',*,*,#5724,.F.);
#7630=ORIENTED_EDGE('',*,*,#5725,.T.);
#7631=ORIENTED_EDGE('',*,*,#5724,.T.);
#7632=ORIENTED_EDGE('',*,*,#5726,.F.);
#7633=ORIENTED_EDGE('',*,*,#5684,.T.);
#7634=ORIENTED_EDGE('',*,*,#5688,.T.);
#7635=ORIENTED_EDGE('',*,*,#5680,.T.);
#7636=ORIENTED_EDGE('',*,*,#5727,.F.);
#7637=ORIENTED_EDGE('',*,*,#5728,.F.);
#7638=ORIENTED_EDGE('',*,*,#5729,.T.);
#7639=ORIENTED_EDGE('',*,*,#5728,.T.);
#7640=ORIENTED_EDGE('',*,*,#5730,.F.);
#7641=ORIENTED_EDGE('',*,*,#5719,.F.);
#7642=ORIENTED_EDGE('',*,*,#5685,.T.);
#7643=ORIENTED_EDGE('',*,*,#5726,.T.);
#7644=ORIENTED_EDGE('',*,*,#5723,.T.);
#7645=ORIENTED_EDGE('',*,*,#5720,.T.);
#7646=ORIENTED_EDGE('',*,*,#5730,.T.);
#7647=ORIENTED_EDGE('',*,*,#5727,.T.);
#7648=ORIENTED_EDGE('',*,*,#5683,.T.);
#7649=ORIENTED_EDGE('',*,*,#5690,.T.);
#7650=ORIENTED_EDGE('',*,*,#5698,.T.);
#7651=ORIENTED_EDGE('',*,*,#5694,.T.);
#7652=ORIENTED_EDGE('',*,*,#5701,.T.);
#7653=ORIENTED_EDGE('',*,*,#5705,.T.);
#7654=ORIENTED_EDGE('',*,*,#5708,.T.);
#7655=ORIENTED_EDGE('',*,*,#5711,.T.);
#7656=ORIENTED_EDGE('',*,*,#5714,.T.);
#7657=ORIENTED_EDGE('',*,*,#5717,.T.);
#7658=ORIENTED_EDGE('',*,*,#5729,.F.);
#7659=ORIENTED_EDGE('',*,*,#5718,.F.);
#7660=ORIENTED_EDGE('',*,*,#5722,.F.);
#7661=ORIENTED_EDGE('',*,*,#5725,.F.);
#7662=ORIENTED_EDGE('',*,*,#5706,.T.);
#7663=ORIENTED_EDGE('',*,*,#5709,.T.);
#7664=ORIENTED_EDGE('',*,*,#5712,.T.);
#7665=ORIENTED_EDGE('',*,*,#5715,.T.);
#7666=ORIENTED_EDGE('',*,*,#5731,.F.);
#7667=ORIENTED_EDGE('',*,*,#5732,.T.);
#7668=ORIENTED_EDGE('',*,*,#5733,.F.);
#7669=ORIENTED_EDGE('',*,*,#5732,.F.);
#7670=ORIENTED_EDGE('',*,*,#5734,.F.);
#7671=ORIENTED_EDGE('',*,*,#5735,.T.);
#7672=ORIENTED_EDGE('',*,*,#5736,.F.);
#7673=ORIENTED_EDGE('',*,*,#5735,.F.);
#7674=ORIENTED_EDGE('',*,*,#5737,.T.);
#7675=ORIENTED_EDGE('',*,*,#5738,.T.);
#7676=ORIENTED_EDGE('',*,*,#5739,.F.);
#7677=ORIENTED_EDGE('',*,*,#5740,.F.);
#7678=ORIENTED_EDGE('',*,*,#5741,.T.);
#7679=ORIENTED_EDGE('',*,*,#5740,.T.);
#7680=ORIENTED_EDGE('',*,*,#5742,.F.);
#7681=ORIENTED_EDGE('',*,*,#5743,.F.);
#7682=ORIENTED_EDGE('',*,*,#5744,.T.);
#7683=ORIENTED_EDGE('',*,*,#5743,.T.);
#7684=ORIENTED_EDGE('',*,*,#5745,.F.);
#7685=ORIENTED_EDGE('',*,*,#5746,.F.);
#7686=ORIENTED_EDGE('',*,*,#5747,.T.);
#7687=ORIENTED_EDGE('',*,*,#5746,.T.);
#7688=ORIENTED_EDGE('',*,*,#5748,.F.);
#7689=ORIENTED_EDGE('',*,*,#5738,.F.);
#7690=ORIENTED_EDGE('',*,*,#5748,.T.);
#7691=ORIENTED_EDGE('',*,*,#5745,.T.);
#7692=ORIENTED_EDGE('',*,*,#5742,.T.);
#7693=ORIENTED_EDGE('',*,*,#5739,.T.);
#7694=ORIENTED_EDGE('',*,*,#5733,.T.);
#7695=ORIENTED_EDGE('',*,*,#5736,.T.);
#7696=ORIENTED_EDGE('',*,*,#5747,.F.);
#7697=ORIENTED_EDGE('',*,*,#5737,.F.);
#7698=ORIENTED_EDGE('',*,*,#5741,.F.);
#7699=ORIENTED_EDGE('',*,*,#5744,.F.);
#7700=ORIENTED_EDGE('',*,*,#5731,.T.);
#7701=ORIENTED_EDGE('',*,*,#5734,.T.);
#7702=ORIENTED_EDGE('',*,*,#5749,.F.);
#7703=ORIENTED_EDGE('',*,*,#5750,.T.);
#7704=ORIENTED_EDGE('',*,*,#5751,.F.);
#7705=ORIENTED_EDGE('',*,*,#5750,.F.);
#7706=ORIENTED_EDGE('',*,*,#5749,.T.);
#7707=ORIENTED_EDGE('',*,*,#5752,.T.);
#7708=ORIENTED_EDGE('',*,*,#5753,.F.);
#7709=ORIENTED_EDGE('',*,*,#5752,.F.);
#7710=ORIENTED_EDGE('',*,*,#5754,.T.);
#7711=ORIENTED_EDGE('',*,*,#5755,.T.);
#7712=ORIENTED_EDGE('',*,*,#5754,.F.);
#7713=ORIENTED_EDGE('',*,*,#5755,.F.);
#7714=ORIENTED_EDGE('',*,*,#5756,.F.);
#7715=ORIENTED_EDGE('',*,*,#5757,.T.);
#7716=ORIENTED_EDGE('',*,*,#5753,.T.);
#7717=ORIENTED_EDGE('',*,*,#5757,.F.);
#7718=ORIENTED_EDGE('',*,*,#5756,.T.);
#7719=ORIENTED_EDGE('',*,*,#5751,.T.);
#7720=ORIENTED_EDGE('',*,*,#5758,.F.);
#7721=ORIENTED_EDGE('',*,*,#5759,.T.);
#7722=ORIENTED_EDGE('',*,*,#5760,.T.);
#7723=ORIENTED_EDGE('',*,*,#5759,.F.);
#7724=ORIENTED_EDGE('',*,*,#5761,.F.);
#7725=ORIENTED_EDGE('',*,*,#5762,.T.);
#7726=ORIENTED_EDGE('',*,*,#5763,.T.);
#7727=ORIENTED_EDGE('',*,*,#5762,.F.);
#7728=ORIENTED_EDGE('',*,*,#5761,.T.);
#7729=ORIENTED_EDGE('',*,*,#5758,.T.);
#7730=ORIENTED_EDGE('',*,*,#5763,.F.);
#7731=ORIENTED_EDGE('',*,*,#5760,.F.);
#7732=ORIENTED_EDGE('',*,*,#5764,.F.);
#7733=ORIENTED_EDGE('',*,*,#5765,.T.);
#7734=ORIENTED_EDGE('',*,*,#5766,.T.);
#7735=ORIENTED_EDGE('',*,*,#5765,.F.);
#7736=ORIENTED_EDGE('',*,*,#5767,.F.);
#7737=ORIENTED_EDGE('',*,*,#5768,.T.);
#7738=ORIENTED_EDGE('',*,*,#5769,.T.);
#7739=ORIENTED_EDGE('',*,*,#5768,.F.);
#7740=ORIENTED_EDGE('',*,*,#5767,.T.);
#7741=ORIENTED_EDGE('',*,*,#5764,.T.);
#7742=ORIENTED_EDGE('',*,*,#5769,.F.);
#7743=ORIENTED_EDGE('',*,*,#5766,.F.);
#7744=ORIENTED_EDGE('',*,*,#5770,.F.);
#7745=ORIENTED_EDGE('',*,*,#5771,.T.);
#7746=ORIENTED_EDGE('',*,*,#5772,.T.);
#7747=ORIENTED_EDGE('',*,*,#5771,.F.);
#7748=ORIENTED_EDGE('',*,*,#5773,.F.);
#7749=ORIENTED_EDGE('',*,*,#5774,.T.);
#7750=ORIENTED_EDGE('',*,*,#5775,.T.);
#7751=ORIENTED_EDGE('',*,*,#5774,.F.);
#7752=ORIENTED_EDGE('',*,*,#5773,.T.);
#7753=ORIENTED_EDGE('',*,*,#5770,.T.);
#7754=ORIENTED_EDGE('',*,*,#5775,.F.);
#7755=ORIENTED_EDGE('',*,*,#5772,.F.);
#7756=ORIENTED_EDGE('',*,*,#5776,.F.);
#7757=ORIENTED_EDGE('',*,*,#5777,.T.);
#7758=ORIENTED_EDGE('',*,*,#5778,.F.);
#7759=ORIENTED_EDGE('',*,*,#5779,.F.);
#7760=ORIENTED_EDGE('',*,*,#5780,.T.);
#7761=ORIENTED_EDGE('',*,*,#5781,.F.);
#7762=ORIENTED_EDGE('',*,*,#5780,.F.);
#7763=ORIENTED_EDGE('',*,*,#5782,.F.);
#7764=ORIENTED_EDGE('',*,*,#5783,.F.);
#7765=ORIENTED_EDGE('',*,*,#5777,.F.);
#7766=ORIENTED_EDGE('',*,*,#5784,.F.);
#7767=ORIENTED_EDGE('',*,*,#5785,.T.);
#7768=ORIENTED_EDGE('',*,*,#5786,.F.);
#7769=ORIENTED_EDGE('',*,*,#5787,.F.);
#7770=ORIENTED_EDGE('',*,*,#5788,.T.);
#7771=ORIENTED_EDGE('',*,*,#5789,.F.);
#7772=ORIENTED_EDGE('',*,*,#5788,.F.);
#7773=ORIENTED_EDGE('',*,*,#5790,.F.);
#7774=ORIENTED_EDGE('',*,*,#5791,.F.);
#7775=ORIENTED_EDGE('',*,*,#5785,.F.);
#7776=ORIENTED_EDGE('',*,*,#5792,.F.);
#7777=ORIENTED_EDGE('',*,*,#5793,.T.);
#7778=ORIENTED_EDGE('',*,*,#5794,.F.);
#7779=ORIENTED_EDGE('',*,*,#5795,.F.);
#7780=ORIENTED_EDGE('',*,*,#5796,.T.);
#7781=ORIENTED_EDGE('',*,*,#5797,.F.);
#7782=ORIENTED_EDGE('',*,*,#5796,.F.);
#7783=ORIENTED_EDGE('',*,*,#5798,.F.);
#7784=ORIENTED_EDGE('',*,*,#5799,.F.);
#7785=ORIENTED_EDGE('',*,*,#5793,.F.);
#7786=ORIENTED_EDGE('',*,*,#5800,.F.);
#7787=ORIENTED_EDGE('',*,*,#5801,.T.);
#7788=ORIENTED_EDGE('',*,*,#5802,.F.);
#7789=ORIENTED_EDGE('',*,*,#5803,.F.);
#7790=ORIENTED_EDGE('',*,*,#5804,.T.);
#7791=ORIENTED_EDGE('',*,*,#5805,.F.);
#7792=ORIENTED_EDGE('',*,*,#5804,.F.);
#7793=ORIENTED_EDGE('',*,*,#5806,.F.);
#7794=ORIENTED_EDGE('',*,*,#5807,.F.);
#7795=ORIENTED_EDGE('',*,*,#5801,.F.);
#7796=ORIENTED_EDGE('',*,*,#5778,.T.);
#7797=ORIENTED_EDGE('',*,*,#5776,.T.);
#7798=ORIENTED_EDGE('',*,*,#5783,.T.);
#7799=ORIENTED_EDGE('',*,*,#5808,.T.);
#7800=ORIENTED_EDGE('',*,*,#5794,.T.);
#7801=ORIENTED_EDGE('',*,*,#5792,.T.);
#7802=ORIENTED_EDGE('',*,*,#5799,.T.);
#7803=ORIENTED_EDGE('',*,*,#5809,.T.);
#7804=ORIENTED_EDGE('',*,*,#5810,.F.);
#7805=ORIENTED_EDGE('',*,*,#5811,.T.);
#7806=ORIENTED_EDGE('',*,*,#5812,.F.);
#7807=ORIENTED_EDGE('',*,*,#5813,.T.);
#7808=ORIENTED_EDGE('',*,*,#5786,.T.);
#7809=ORIENTED_EDGE('',*,*,#5784,.T.);
#7810=ORIENTED_EDGE('',*,*,#5791,.T.);
#7811=ORIENTED_EDGE('',*,*,#5814,.T.);
#7812=ORIENTED_EDGE('',*,*,#5802,.T.);
#7813=ORIENTED_EDGE('',*,*,#5800,.T.);
#7814=ORIENTED_EDGE('',*,*,#5807,.T.);
#7815=ORIENTED_EDGE('',*,*,#5815,.T.);
#7816=ORIENTED_EDGE('',*,*,#5816,.F.);
#7817=ORIENTED_EDGE('',*,*,#5817,.F.);
#7818=ORIENTED_EDGE('',*,*,#5818,.F.);
#7819=ORIENTED_EDGE('',*,*,#5819,.T.);
#7820=ORIENTED_EDGE('',*,*,#5810,.T.);
#7821=ORIENTED_EDGE('',*,*,#5820,.T.);
#7822=ORIENTED_EDGE('',*,*,#5821,.T.);
#7823=ORIENTED_EDGE('',*,*,#5822,.T.);
#7824=ORIENTED_EDGE('',*,*,#5823,.T.);
#7825=ORIENTED_EDGE('',*,*,#5824,.T.);
#7826=ORIENTED_EDGE('',*,*,#5818,.T.);
#7827=ORIENTED_EDGE('',*,*,#5825,.T.);
#7828=ORIENTED_EDGE('',*,*,#5826,.T.);
#7829=ORIENTED_EDGE('',*,*,#5827,.T.);
#7830=ORIENTED_EDGE('',*,*,#5828,.T.);
#7831=ORIENTED_EDGE('',*,*,#5829,.T.);
#7832=ORIENTED_EDGE('',*,*,#5782,.T.);
#7833=ORIENTED_EDGE('',*,*,#5779,.T.);
#7834=ORIENTED_EDGE('',*,*,#5813,.F.);
#7835=ORIENTED_EDGE('',*,*,#5830,.F.);
#7836=ORIENTED_EDGE('',*,*,#5831,.F.);
#7837=ORIENTED_EDGE('',*,*,#5820,.F.);
#7838=ORIENTED_EDGE('',*,*,#5809,.F.);
#7839=ORIENTED_EDGE('',*,*,#5798,.T.);
#7840=ORIENTED_EDGE('',*,*,#5795,.T.);
#7841=ORIENTED_EDGE('',*,*,#5808,.F.);
#7842=ORIENTED_EDGE('',*,*,#5831,.T.);
#7843=ORIENTED_EDGE('',*,*,#5832,.F.);
#7844=ORIENTED_EDGE('',*,*,#5833,.F.);
#7845=ORIENTED_EDGE('',*,*,#5821,.F.);
#7846=ORIENTED_EDGE('',*,*,#5833,.T.);
#7847=ORIENTED_EDGE('',*,*,#5834,.F.);
#7848=ORIENTED_EDGE('',*,*,#5835,.F.);
#7849=ORIENTED_EDGE('',*,*,#5822,.F.);
#7850=ORIENTED_EDGE('',*,*,#5781,.T.);
#7851=ORIENTED_EDGE('',*,*,#5789,.T.);
#7852=ORIENTED_EDGE('',*,*,#5797,.T.);
#7853=ORIENTED_EDGE('',*,*,#5805,.T.);
#7854=ORIENTED_EDGE('',*,*,#5835,.T.);
#7855=ORIENTED_EDGE('',*,*,#5836,.F.);
#7856=ORIENTED_EDGE('',*,*,#5837,.F.);
#7857=ORIENTED_EDGE('',*,*,#5823,.F.);
#7858=ORIENTED_EDGE('',*,*,#5790,.T.);
#7859=ORIENTED_EDGE('',*,*,#5787,.T.);
#7860=ORIENTED_EDGE('',*,*,#5819,.F.);
#7861=ORIENTED_EDGE('',*,*,#5824,.F.);
#7862=ORIENTED_EDGE('',*,*,#5837,.T.);
#7863=ORIENTED_EDGE('',*,*,#5838,.F.);
#7864=ORIENTED_EDGE('',*,*,#5815,.F.);
#7865=ORIENTED_EDGE('',*,*,#5806,.T.);
#7866=ORIENTED_EDGE('',*,*,#5803,.T.);
#7867=ORIENTED_EDGE('',*,*,#5814,.F.);
#7868=ORIENTED_EDGE('',*,*,#5817,.T.);
#7869=ORIENTED_EDGE('',*,*,#5839,.F.);
#7870=ORIENTED_EDGE('',*,*,#5840,.F.);
#7871=ORIENTED_EDGE('',*,*,#5825,.F.);
#7872=ORIENTED_EDGE('',*,*,#5840,.T.);
#7873=ORIENTED_EDGE('',*,*,#5841,.F.);
#7874=ORIENTED_EDGE('',*,*,#5842,.F.);
#7875=ORIENTED_EDGE('',*,*,#5826,.F.);
#7876=ORIENTED_EDGE('',*,*,#5842,.T.);
#7877=ORIENTED_EDGE('',*,*,#5843,.F.);
#7878=ORIENTED_EDGE('',*,*,#5844,.F.);
#7879=ORIENTED_EDGE('',*,*,#5827,.F.);
#7880=ORIENTED_EDGE('',*,*,#5844,.T.);
#7881=ORIENTED_EDGE('',*,*,#5845,.F.);
#7882=ORIENTED_EDGE('',*,*,#5846,.F.);
#7883=ORIENTED_EDGE('',*,*,#5828,.F.);
#7884=ORIENTED_EDGE('',*,*,#5846,.T.);
#7885=ORIENTED_EDGE('',*,*,#5847,.F.);
#7886=ORIENTED_EDGE('',*,*,#5811,.F.);
#7887=ORIENTED_EDGE('',*,*,#5829,.F.);
#7888=ORIENTED_EDGE('',*,*,#5812,.T.);
#7889=ORIENTED_EDGE('',*,*,#5847,.T.);
#7890=ORIENTED_EDGE('',*,*,#5845,.T.);
#7891=ORIENTED_EDGE('',*,*,#5843,.T.);
#7892=ORIENTED_EDGE('',*,*,#5841,.T.);
#7893=ORIENTED_EDGE('',*,*,#5839,.T.);
#7894=ORIENTED_EDGE('',*,*,#5816,.T.);
#7895=ORIENTED_EDGE('',*,*,#5838,.T.);
#7896=ORIENTED_EDGE('',*,*,#5836,.T.);
#7897=ORIENTED_EDGE('',*,*,#5834,.T.);
#7898=ORIENTED_EDGE('',*,*,#5832,.T.);
#7899=ORIENTED_EDGE('',*,*,#5830,.T.);
#7900=ORIENTED_EDGE('',*,*,#5848,.T.);
#7901=ORIENTED_EDGE('',*,*,#5849,.T.);
#7902=ORIENTED_EDGE('',*,*,#5850,.F.);
#7903=ORIENTED_EDGE('',*,*,#5851,.F.);
#7904=ORIENTED_EDGE('',*,*,#5852,.T.);
#7905=ORIENTED_EDGE('',*,*,#5851,.T.);
#7906=ORIENTED_EDGE('',*,*,#5853,.F.);
#7907=ORIENTED_EDGE('',*,*,#5854,.F.);
#7908=ORIENTED_EDGE('',*,*,#5855,.T.);
#7909=ORIENTED_EDGE('',*,*,#5854,.T.);
#7910=ORIENTED_EDGE('',*,*,#5856,.F.);
#7911=ORIENTED_EDGE('',*,*,#5857,.F.);
#7912=ORIENTED_EDGE('',*,*,#5858,.T.);
#7913=ORIENTED_EDGE('',*,*,#5857,.T.);
#7914=ORIENTED_EDGE('',*,*,#5859,.F.);
#7915=ORIENTED_EDGE('',*,*,#5860,.F.);
#7916=ORIENTED_EDGE('',*,*,#5861,.T.);
#7917=ORIENTED_EDGE('',*,*,#5860,.T.);
#7918=ORIENTED_EDGE('',*,*,#5862,.F.);
#7919=ORIENTED_EDGE('',*,*,#5863,.F.);
#7920=ORIENTED_EDGE('',*,*,#5864,.T.);
#7921=ORIENTED_EDGE('',*,*,#5863,.T.);
#7922=ORIENTED_EDGE('',*,*,#5865,.F.);
#7923=ORIENTED_EDGE('',*,*,#5866,.F.);
#7924=ORIENTED_EDGE('',*,*,#5867,.T.);
#7925=ORIENTED_EDGE('',*,*,#5866,.T.);
#7926=ORIENTED_EDGE('',*,*,#5868,.F.);
#7927=ORIENTED_EDGE('',*,*,#5869,.F.);
#7928=ORIENTED_EDGE('',*,*,#5870,.T.);
#7929=ORIENTED_EDGE('',*,*,#5869,.T.);
#7930=ORIENTED_EDGE('',*,*,#5871,.F.);
#7931=ORIENTED_EDGE('',*,*,#5849,.F.);
#7932=ORIENTED_EDGE('',*,*,#5871,.T.);
#7933=ORIENTED_EDGE('',*,*,#5868,.T.);
#7934=ORIENTED_EDGE('',*,*,#5865,.T.);
#7935=ORIENTED_EDGE('',*,*,#5862,.T.);
#7936=ORIENTED_EDGE('',*,*,#5859,.T.);
#7937=ORIENTED_EDGE('',*,*,#5856,.T.);
#7938=ORIENTED_EDGE('',*,*,#5853,.T.);
#7939=ORIENTED_EDGE('',*,*,#5850,.T.);
#7940=ORIENTED_EDGE('',*,*,#5870,.F.);
#7941=ORIENTED_EDGE('',*,*,#5848,.F.);
#7942=ORIENTED_EDGE('',*,*,#5852,.F.);
#7943=ORIENTED_EDGE('',*,*,#5855,.F.);
#7944=ORIENTED_EDGE('',*,*,#5858,.F.);
#7945=ORIENTED_EDGE('',*,*,#5861,.F.);
#7946=ORIENTED_EDGE('',*,*,#5864,.F.);
#7947=ORIENTED_EDGE('',*,*,#5867,.F.);
#7948=ORIENTED_EDGE('',*,*,#5872,.F.);
#7949=ORIENTED_EDGE('',*,*,#5873,.T.);
#7950=ORIENTED_EDGE('',*,*,#5874,.F.);
#7951=ORIENTED_EDGE('',*,*,#5875,.F.);
#7952=ORIENTED_EDGE('',*,*,#5876,.F.);
#7953=ORIENTED_EDGE('',*,*,#5875,.T.);
#7954=ORIENTED_EDGE('',*,*,#5877,.F.);
#7955=ORIENTED_EDGE('',*,*,#5878,.F.);
#7956=ORIENTED_EDGE('',*,*,#5879,.F.);
#7957=ORIENTED_EDGE('',*,*,#5878,.T.);
#7958=ORIENTED_EDGE('',*,*,#5880,.F.);
#7959=ORIENTED_EDGE('',*,*,#5881,.F.);
#7960=ORIENTED_EDGE('',*,*,#5882,.F.);
#7961=ORIENTED_EDGE('',*,*,#5881,.T.);
#7962=ORIENTED_EDGE('',*,*,#5883,.F.);
#7963=ORIENTED_EDGE('',*,*,#5884,.F.);
#7964=ORIENTED_EDGE('',*,*,#5885,.F.);
#7965=ORIENTED_EDGE('',*,*,#5884,.T.);
#7966=ORIENTED_EDGE('',*,*,#5886,.F.);
#7967=ORIENTED_EDGE('',*,*,#5887,.F.);
#7968=ORIENTED_EDGE('',*,*,#5888,.F.);
#7969=ORIENTED_EDGE('',*,*,#5887,.T.);
#7970=ORIENTED_EDGE('',*,*,#5889,.F.);
#7971=ORIENTED_EDGE('',*,*,#5890,.F.);
#7972=ORIENTED_EDGE('',*,*,#5891,.F.);
#7973=ORIENTED_EDGE('',*,*,#5890,.T.);
#7974=ORIENTED_EDGE('',*,*,#5892,.F.);
#7975=ORIENTED_EDGE('',*,*,#5893,.F.);
#7976=ORIENTED_EDGE('',*,*,#5894,.F.);
#7977=ORIENTED_EDGE('',*,*,#5893,.T.);
#7978=ORIENTED_EDGE('',*,*,#5895,.F.);
#7979=ORIENTED_EDGE('',*,*,#5873,.F.);
#7980=ORIENTED_EDGE('',*,*,#5894,.T.);
#7981=ORIENTED_EDGE('',*,*,#5872,.T.);
#7982=ORIENTED_EDGE('',*,*,#5876,.T.);
#7983=ORIENTED_EDGE('',*,*,#5879,.T.);
#7984=ORIENTED_EDGE('',*,*,#5882,.T.);
#7985=ORIENTED_EDGE('',*,*,#5885,.T.);
#7986=ORIENTED_EDGE('',*,*,#5888,.T.);
#7987=ORIENTED_EDGE('',*,*,#5891,.T.);
#7988=ORIENTED_EDGE('',*,*,#5895,.T.);
#7989=ORIENTED_EDGE('',*,*,#5892,.T.);
#7990=ORIENTED_EDGE('',*,*,#5889,.T.);
#7991=ORIENTED_EDGE('',*,*,#5886,.T.);
#7992=ORIENTED_EDGE('',*,*,#5883,.T.);
#7993=ORIENTED_EDGE('',*,*,#5880,.T.);
#7994=ORIENTED_EDGE('',*,*,#5877,.T.);
#7995=ORIENTED_EDGE('',*,*,#5874,.T.);
#7996=ORIENTED_EDGE('',*,*,#5896,.T.);
#7997=ORIENTED_EDGE('',*,*,#5897,.T.);
#7998=ORIENTED_EDGE('',*,*,#5898,.T.);
#7999=ORIENTED_EDGE('',*,*,#5899,.F.);
#8000=ORIENTED_EDGE('',*,*,#5900,.T.);
#8001=ORIENTED_EDGE('',*,*,#5901,.T.);
#8002=ORIENTED_EDGE('',*,*,#5902,.T.);
#8003=ORIENTED_EDGE('',*,*,#5897,.F.);
#8004=ORIENTED_EDGE('',*,*,#5903,.T.);
#8005=ORIENTED_EDGE('',*,*,#5904,.T.);
#8006=ORIENTED_EDGE('',*,*,#5905,.T.);
#8007=ORIENTED_EDGE('',*,*,#5901,.F.);
#8008=ORIENTED_EDGE('',*,*,#5906,.T.);
#8009=ORIENTED_EDGE('',*,*,#5907,.T.);
#8010=ORIENTED_EDGE('',*,*,#5908,.T.);
#8011=ORIENTED_EDGE('',*,*,#5904,.F.);
#8012=ORIENTED_EDGE('',*,*,#5909,.T.);
#8013=ORIENTED_EDGE('',*,*,#5910,.T.);
#8014=ORIENTED_EDGE('',*,*,#5911,.T.);
#8015=ORIENTED_EDGE('',*,*,#5907,.F.);
#8016=ORIENTED_EDGE('',*,*,#5912,.T.);
#8017=ORIENTED_EDGE('',*,*,#5899,.T.);
#8018=ORIENTED_EDGE('',*,*,#5913,.T.);
#8019=ORIENTED_EDGE('',*,*,#5910,.F.);
#8020=ORIENTED_EDGE('',*,*,#5912,.F.);
#8021=ORIENTED_EDGE('',*,*,#5909,.F.);
#8022=ORIENTED_EDGE('',*,*,#5906,.F.);
#8023=ORIENTED_EDGE('',*,*,#5903,.F.);
#8024=ORIENTED_EDGE('',*,*,#5900,.F.);
#8025=ORIENTED_EDGE('',*,*,#5896,.F.);
#8026=ORIENTED_EDGE('',*,*,#5913,.F.);
#8027=ORIENTED_EDGE('',*,*,#5898,.F.);
#8028=ORIENTED_EDGE('',*,*,#5902,.F.);
#8029=ORIENTED_EDGE('',*,*,#5905,.F.);
#8030=ORIENTED_EDGE('',*,*,#5908,.F.);
#8031=ORIENTED_EDGE('',*,*,#5911,.F.);
#8032=ORIENTED_EDGE('',*,*,#5914,.F.);
#8033=ORIENTED_EDGE('',*,*,#5915,.F.);
#8034=ORIENTED_EDGE('',*,*,#5916,.F.);
#8035=ORIENTED_EDGE('',*,*,#5917,.T.);
#8036=ORIENTED_EDGE('',*,*,#5915,.T.);
#8037=ORIENTED_EDGE('',*,*,#5917,.F.);
#8038=ORIENTED_EDGE('',*,*,#5918,.F.);
#8039=ORIENTED_EDGE('',*,*,#5919,.T.);
#8040=ORIENTED_EDGE('',*,*,#5916,.T.);
#8041=ORIENTED_EDGE('',*,*,#5919,.F.);
#8042=ORIENTED_EDGE('',*,*,#5920,.F.);
#8043=ORIENTED_EDGE('',*,*,#5921,.T.);
#8044=ORIENTED_EDGE('',*,*,#5918,.T.);
#8045=ORIENTED_EDGE('',*,*,#5921,.F.);
#8046=ORIENTED_EDGE('',*,*,#5920,.T.);
#8047=ORIENTED_EDGE('',*,*,#5922,.F.);
#8048=ORIENTED_EDGE('',*,*,#5923,.F.);
#8049=ORIENTED_EDGE('',*,*,#5924,.T.);
#8050=ORIENTED_EDGE('',*,*,#5922,.T.);
#8051=ORIENTED_EDGE('',*,*,#5924,.F.);
#8052=ORIENTED_EDGE('',*,*,#5914,.T.);
#8053=ORIENTED_EDGE('',*,*,#5925,.T.);
#8054=ORIENTED_EDGE('',*,*,#5923,.T.);
#8055=ORIENTED_EDGE('',*,*,#5925,.F.);
#8056=ORIENTED_EDGE('',*,*,#5926,.T.);
#8057=ORIENTED_EDGE('',*,*,#5927,.T.);
#8058=ORIENTED_EDGE('',*,*,#5928,.T.);
#8059=ORIENTED_EDGE('',*,*,#5927,.F.);
#8060=ORIENTED_EDGE('',*,*,#5928,.F.);
#8061=ORIENTED_EDGE('',*,*,#5929,.T.);
#8062=ORIENTED_EDGE('',*,*,#5930,.T.);
#8063=ORIENTED_EDGE('',*,*,#5929,.F.);
#8064=ORIENTED_EDGE('',*,*,#5931,.T.);
#8065=ORIENTED_EDGE('',*,*,#5926,.F.);
#8066=ORIENTED_EDGE('',*,*,#5931,.F.);
#8067=ORIENTED_EDGE('',*,*,#5932,.T.);
#8068=ORIENTED_EDGE('',*,*,#5933,.T.);
#8069=ORIENTED_EDGE('',*,*,#5932,.F.);
#8070=ORIENTED_EDGE('',*,*,#5933,.F.);
#8071=ORIENTED_EDGE('',*,*,#5930,.F.);
#8072=ORIENTED_EDGE('',*,*,#5934,.F.);
#8073=ORIENTED_EDGE('',*,*,#5935,.F.);
#8074=ORIENTED_EDGE('',*,*,#5936,.T.);
#8075=ORIENTED_EDGE('',*,*,#5934,.T.);
#8076=ORIENTED_EDGE('',*,*,#5936,.F.);
#8077=ORIENTED_EDGE('',*,*,#5937,.F.);
#8078=ORIENTED_EDGE('',*,*,#5938,.T.);
#8079=ORIENTED_EDGE('',*,*,#5935,.T.);
#8080=ORIENTED_EDGE('',*,*,#5938,.F.);
#8081=ORIENTED_EDGE('',*,*,#5939,.F.);
#8082=ORIENTED_EDGE('',*,*,#5940,.T.);
#8083=ORIENTED_EDGE('',*,*,#5937,.T.);
#8084=ORIENTED_EDGE('',*,*,#5940,.F.);
#8085=ORIENTED_EDGE('',*,*,#5939,.T.);
#8086=ORIENTED_EDGE('',*,*,#5941,.F.);
#8087=ORIENTED_EDGE('',*,*,#5942,.F.);
#8088=ORIENTED_EDGE('',*,*,#5943,.T.);
#8089=ORIENTED_EDGE('',*,*,#5941,.T.);
#8090=ORIENTED_EDGE('',*,*,#5943,.F.);
#8091=ORIENTED_EDGE('',*,*,#5944,.F.);
#8092=ORIENTED_EDGE('',*,*,#5945,.T.);
#8093=ORIENTED_EDGE('',*,*,#5942,.T.);
#8094=ORIENTED_EDGE('',*,*,#5945,.F.);
#8095=ORIENTED_EDGE('',*,*,#5946,.F.);
#8096=ORIENTED_EDGE('',*,*,#5947,.T.);
#8097=ORIENTED_EDGE('',*,*,#5944,.T.);
#8098=ORIENTED_EDGE('',*,*,#5947,.F.);
#8099=ORIENTED_EDGE('',*,*,#5946,.T.);
#8100=ORIENTED_EDGE('',*,*,#5948,.T.);
#8101=ORIENTED_EDGE('',*,*,#5949,.T.);
#8102=ORIENTED_EDGE('',*,*,#5950,.T.);
#8103=ORIENTED_EDGE('',*,*,#5951,.F.);
#8104=ORIENTED_EDGE('',*,*,#5952,.T.);
#8105=ORIENTED_EDGE('',*,*,#5953,.T.);
#8106=ORIENTED_EDGE('',*,*,#5954,.T.);
#8107=ORIENTED_EDGE('',*,*,#5949,.F.);
#8108=ORIENTED_EDGE('',*,*,#5955,.T.);
#8109=ORIENTED_EDGE('',*,*,#5956,.T.);
#8110=ORIENTED_EDGE('',*,*,#5957,.T.);
#8111=ORIENTED_EDGE('',*,*,#5953,.F.);
#8112=ORIENTED_EDGE('',*,*,#5958,.T.);
#8113=ORIENTED_EDGE('',*,*,#5959,.T.);
#8114=ORIENTED_EDGE('',*,*,#5960,.T.);
#8115=ORIENTED_EDGE('',*,*,#5956,.F.);
#8116=ORIENTED_EDGE('',*,*,#5961,.T.);
#8117=ORIENTED_EDGE('',*,*,#5962,.T.);
#8118=ORIENTED_EDGE('',*,*,#5963,.T.);
#8119=ORIENTED_EDGE('',*,*,#5959,.F.);
#8120=ORIENTED_EDGE('',*,*,#5964,.T.);
#8121=ORIENTED_EDGE('',*,*,#5951,.T.);
#8122=ORIENTED_EDGE('',*,*,#5965,.T.);
#8123=ORIENTED_EDGE('',*,*,#5962,.F.);
#8124=ORIENTED_EDGE('',*,*,#5964,.F.);
#8125=ORIENTED_EDGE('',*,*,#5961,.F.);
#8126=ORIENTED_EDGE('',*,*,#5958,.F.);
#8127=ORIENTED_EDGE('',*,*,#5955,.F.);
#8128=ORIENTED_EDGE('',*,*,#5952,.F.);
#8129=ORIENTED_EDGE('',*,*,#5948,.F.);
#8130=ORIENTED_EDGE('',*,*,#5965,.F.);
#8131=ORIENTED_EDGE('',*,*,#5950,.F.);
#8132=ORIENTED_EDGE('',*,*,#5954,.F.);
#8133=ORIENTED_EDGE('',*,*,#5957,.F.);
#8134=ORIENTED_EDGE('',*,*,#5960,.F.);
#8135=ORIENTED_EDGE('',*,*,#5963,.F.);
#8136=ORIENTED_EDGE('',*,*,#5966,.T.);
#8137=ORIENTED_EDGE('',*,*,#5967,.T.);
#8138=ORIENTED_EDGE('',*,*,#5968,.T.);
#8139=ORIENTED_EDGE('',*,*,#5969,.F.);
#8140=ORIENTED_EDGE('',*,*,#5970,.T.);
#8141=ORIENTED_EDGE('',*,*,#5971,.T.);
#8142=ORIENTED_EDGE('',*,*,#5972,.T.);
#8143=ORIENTED_EDGE('',*,*,#5967,.F.);
#8144=ORIENTED_EDGE('',*,*,#5973,.T.);
#8145=ORIENTED_EDGE('',*,*,#5974,.T.);
#8146=ORIENTED_EDGE('',*,*,#5975,.T.);
#8147=ORIENTED_EDGE('',*,*,#5971,.F.);
#8148=ORIENTED_EDGE('',*,*,#5976,.T.);
#8149=ORIENTED_EDGE('',*,*,#5977,.T.);
#8150=ORIENTED_EDGE('',*,*,#5978,.T.);
#8151=ORIENTED_EDGE('',*,*,#5974,.F.);
#8152=ORIENTED_EDGE('',*,*,#5979,.T.);
#8153=ORIENTED_EDGE('',*,*,#5980,.T.);
#8154=ORIENTED_EDGE('',*,*,#5981,.T.);
#8155=ORIENTED_EDGE('',*,*,#5977,.F.);
#8156=ORIENTED_EDGE('',*,*,#5982,.T.);
#8157=ORIENTED_EDGE('',*,*,#5969,.T.);
#8158=ORIENTED_EDGE('',*,*,#5983,.T.);
#8159=ORIENTED_EDGE('',*,*,#5980,.F.);
#8160=ORIENTED_EDGE('',*,*,#5982,.F.);
#8161=ORIENTED_EDGE('',*,*,#5979,.F.);
#8162=ORIENTED_EDGE('',*,*,#5976,.F.);
#8163=ORIENTED_EDGE('',*,*,#5973,.F.);
#8164=ORIENTED_EDGE('',*,*,#5970,.F.);
#8165=ORIENTED_EDGE('',*,*,#5966,.F.);
#8166=ORIENTED_EDGE('',*,*,#5983,.F.);
#8167=ORIENTED_EDGE('',*,*,#5968,.F.);
#8168=ORIENTED_EDGE('',*,*,#5972,.F.);
#8169=ORIENTED_EDGE('',*,*,#5975,.F.);
#8170=ORIENTED_EDGE('',*,*,#5978,.F.);
#8171=ORIENTED_EDGE('',*,*,#5981,.F.);
#8172=ORIENTED_EDGE('',*,*,#5984,.F.);
#8173=ORIENTED_EDGE('',*,*,#5985,.F.);
#8174=ORIENTED_EDGE('',*,*,#5986,.F.);
#8175=ORIENTED_EDGE('',*,*,#5987,.T.);
#8176=ORIENTED_EDGE('',*,*,#5985,.T.);
#8177=ORIENTED_EDGE('',*,*,#5987,.F.);
#8178=ORIENTED_EDGE('',*,*,#5988,.F.);
#8179=ORIENTED_EDGE('',*,*,#5989,.T.);
#8180=ORIENTED_EDGE('',*,*,#5986,.T.);
#8181=ORIENTED_EDGE('',*,*,#5989,.F.);
#8182=ORIENTED_EDGE('',*,*,#5990,.F.);
#8183=ORIENTED_EDGE('',*,*,#5991,.T.);
#8184=ORIENTED_EDGE('',*,*,#5988,.T.);
#8185=ORIENTED_EDGE('',*,*,#5991,.F.);
#8186=ORIENTED_EDGE('',*,*,#5990,.T.);
#8187=ORIENTED_EDGE('',*,*,#5992,.F.);
#8188=ORIENTED_EDGE('',*,*,#5993,.F.);
#8189=ORIENTED_EDGE('',*,*,#5994,.T.);
#8190=ORIENTED_EDGE('',*,*,#5992,.T.);
#8191=ORIENTED_EDGE('',*,*,#5994,.F.);
#8192=ORIENTED_EDGE('',*,*,#5984,.T.);
#8193=ORIENTED_EDGE('',*,*,#5995,.T.);
#8194=ORIENTED_EDGE('',*,*,#5993,.T.);
#8195=ORIENTED_EDGE('',*,*,#5995,.F.);
#8196=CYLINDRICAL_SURFACE('',#9496,0.210000000000001);
#8197=CYLINDRICAL_SURFACE('',#9499,0.21);
#8198=CYLINDRICAL_SURFACE('',#9502,0.21);
#8199=CYLINDRICAL_SURFACE('',#9505,0.210000000000001);
#8200=CYLINDRICAL_SURFACE('',#9508,0.21);
#8201=CYLINDRICAL_SURFACE('',#9511,0.21);
#8202=CYLINDRICAL_SURFACE('',#9514,0.21);
#8203=CYLINDRICAL_SURFACE('',#9517,0.21);
#8204=CYLINDRICAL_SURFACE('',#9520,0.21);
#8205=CYLINDRICAL_SURFACE('',#9523,0.21);
#8206=CYLINDRICAL_SURFACE('',#9526,0.21);
#8207=CYLINDRICAL_SURFACE('',#9529,0.21);
#8208=CYLINDRICAL_SURFACE('',#9539,0.34);
#8209=CYLINDRICAL_SURFACE('',#9543,0.34);
#8210=CYLINDRICAL_SURFACE('',#9547,0.5);
#8211=CYLINDRICAL_SURFACE('',#9552,0.5);
#8212=CYLINDRICAL_SURFACE('',#9557,0.5);
#8213=CYLINDRICAL_SURFACE('',#9562,0.5);
#8214=CYLINDRICAL_SURFACE('',#9567,0.275);
#8215=CYLINDRICAL_SURFACE('',#9569,0.275);
#8216=CYLINDRICAL_SURFACE('',#9571,0.275);
#8217=CYLINDRICAL_SURFACE('',#9573,0.275);
#8218=CYLINDRICAL_SURFACE('',#9582,0.425);
#8219=CYLINDRICAL_SURFACE('',#9585,0.645);
#8220=CYLINDRICAL_SURFACE('',#9591,0.425);
#8221=CYLINDRICAL_SURFACE('',#9594,0.645);
#8222=CYLINDRICAL_SURFACE('',#9600,0.34);
#8223=CYLINDRICAL_SURFACE('',#9604,0.34);
#8224=CYLINDRICAL_SURFACE('',#9608,0.5);
#8225=CYLINDRICAL_SURFACE('',#9613,0.5);
#8226=CYLINDRICAL_SURFACE('',#9618,0.5);
#8227=CYLINDRICAL_SURFACE('',#9623,0.5);
#8228=CYLINDRICAL_SURFACE('',#9628,0.275);
#8229=CYLINDRICAL_SURFACE('',#9630,0.275);
#8230=CYLINDRICAL_SURFACE('',#9632,0.275);
#8231=CYLINDRICAL_SURFACE('',#9634,0.275);
#8232=CYLINDRICAL_SURFACE('',#9643,0.425);
#8233=CYLINDRICAL_SURFACE('',#9646,0.645);
#8234=CYLINDRICAL_SURFACE('',#9652,0.425);
#8235=CYLINDRICAL_SURFACE('',#9655,0.645);
#8236=CYLINDRICAL_SURFACE('',#9661,0.164999999999999);
#8237=CYLINDRICAL_SURFACE('',#9665,0.164999999999999);
#8238=CYLINDRICAL_SURFACE('',#9669,0.165);
#8239=CYLINDRICAL_SURFACE('',#9673,0.164999999999999);
#8240=CYLINDRICAL_SURFACE('',#9677,0.5);
#8241=CYLINDRICAL_SURFACE('',#9682,0.5);
#8242=CYLINDRICAL_SURFACE('',#9687,0.5);
#8243=CYLINDRICAL_SURFACE('',#9692,0.5);
#8244=CYLINDRICAL_SURFACE('',#9697,0.274999999999999);
#8245=CYLINDRICAL_SURFACE('',#9699,0.275);
#8246=CYLINDRICAL_SURFACE('',#9701,0.275);
#8247=CYLINDRICAL_SURFACE('',#9703,0.274999999999999);
#8248=CYLINDRICAL_SURFACE('',#9727,2.05);
#8249=CYLINDRICAL_SURFACE('',#9730,2.05);
#8250=CYLINDRICAL_SURFACE('',#9748,2.8);
#8251=CYLINDRICAL_SURFACE('',#9758,0.65);
#8252=CYLINDRICAL_SURFACE('',#9760,0.65);
#8253=CYLINDRICAL_SURFACE('',#9768,1.8);
#8254=CYLINDRICAL_SURFACE('',#9777,0.25);
#8255=CYLINDRICAL_SURFACE('',#9778,0.25);
#8256=CYLINDRICAL_SURFACE('',#9779,1.65);
#8257=CYLINDRICAL_SURFACE('',#9782,0.25);
#8258=CYLINDRICAL_SURFACE('',#9783,0.25);
#8259=CYLINDRICAL_SURFACE('',#9784,0.25);
#8260=CYLINDRICAL_SURFACE('',#9785,0.25);
#8261=CYLINDRICAL_SURFACE('',#9790,1.75);
#8262=CYLINDRICAL_SURFACE('',#9794,1.);
#8263=CYLINDRICAL_SURFACE('',#9798,0.42);
#8264=CYLINDRICAL_SURFACE('',#9801,0.8);
#8265=CYLINDRICAL_SURFACE('',#9821,0.65);
#8266=CYLINDRICAL_SURFACE('',#9829,0.3933);
#8267=CYLINDRICAL_SURFACE('',#9831,0.375);
#8268=CYLINDRICAL_SURFACE('',#9836,0.375);
#8269=CYLINDRICAL_SURFACE('',#9841,0.375);
#8270=CYLINDRICAL_SURFACE('',#9846,0.375);
#8271=CYLINDRICAL_SURFACE('',#9851,0.225);
#8272=CYLINDRICAL_SURFACE('',#9853,0.225);
#8273=CYLINDRICAL_SURFACE('',#9855,0.225);
#8274=CYLINDRICAL_SURFACE('',#9857,0.225000000000001);
#8275=CYLINDRICAL_SURFACE('',#9878,0.35);
#8276=CYLINDRICAL_SURFACE('',#9886,0.1954);
#8277=CYLINDRICAL_SURFACE('',#9906,1.);
#8278=CYLINDRICAL_SURFACE('',#9915,0.21);
#8279=CYLINDRICAL_SURFACE('',#9919,1.005);
#8280=CYLINDRICAL_SURFACE('',#9922,1.5);
#8281=CYLINDRICAL_SURFACE('',#9930,0.21);
#8282=CYLINDRICAL_SURFACE('',#9934,1.005);
#8283=CYLINDRICAL_SURFACE('',#9937,1.5);
#8284=CYLINDRICAL_SURFACE('',#9943,1.005);
#8285=CYLINDRICAL_SURFACE('',#9946,1.3);
#8286=CYLINDRICAL_SURFACE('',#9955,0.34);
#8287=CYLINDRICAL_SURFACE('',#9959,1.);
#8288=CYLINDRICAL_SURFACE('',#9971,0.21);
#8289=CYLINDRICAL_SURFACE('',#9978,4.);
#8290=CYLINDRICAL_SURFACE('',#9979,1.6);
#8291=CYLINDRICAL_SURFACE('',#9984,0.165);
#8292=CYLINDRICAL_SURFACE('',#9991,0.5);
#8293=CYLINDRICAL_SURFACE('',#9994,0.4);
#8294=CYLINDRICAL_SURFACE('',#9998,0.505);
#8295=CYLINDRICAL_SURFACE('',#10001,0.7);
#8296=CYLINDRICAL_SURFACE('',#10007,0.505);
#8297=CYLINDRICAL_SURFACE('',#10010,0.7);
#8298=CYLINDRICAL_SURFACE('',#10016,0.225);
#8299=CYLINDRICAL_SURFACE('',#10019,0.8);
#8300=CYLINDRICAL_SURFACE('',#10047,0.24505);
#8301=CYLINDRICAL_SURFACE('',#10054,1.5);
#8302=CYLINDRICAL_SURFACE('',#10057,1.5);
#8303=CYLINDRICAL_SURFACE('',#10060,2.);
#8304=CYLINDRICAL_SURFACE('',#10066,2.);
#8305=CYLINDRICAL_SURFACE('',#10071,1.1);
#8306=CYLINDRICAL_SURFACE('',#10074,2.);
#8307=CYLINDRICAL_SURFACE('',#10080,1.1);
#8308=CYLINDRICAL_SURFACE('',#10083,2.);
#8309=CYLINDRICAL_SURFACE('',#10089,1.1);
#8310=CYLINDRICAL_SURFACE('',#10092,2.);
#8311=CYLINDRICAL_SURFACE('',#10098,1.1);
#8312=CYLINDRICAL_SURFACE('',#10101,2.);
#8313=CYLINDRICAL_SURFACE('',#10114,0.976185);
#8314=CYLINDRICAL_SURFACE('',#10116,0.5);
#8315=CYLINDRICAL_SURFACE('',#10122,0.976185);
#8316=CYLINDRICAL_SURFACE('',#10134,1.023815);
#8317=CYLINDRICAL_SURFACE('',#10141,1.5);
#8318=CYLINDRICAL_SURFACE('',#10146,1.023815);
#8319=CYLINDRICAL_SURFACE('',#10168,1.019052);
#8320=CYLINDRICAL_SURFACE('',#10208,0.980948);
#8321=CYLINDRICAL_SURFACE('',#10222,1.013815);
#8322=CYLINDRICAL_SURFACE('',#10226,0.991185);
#8323=CYLINDRICAL_SURFACE('',#10230,1.013815);
#8324=CYLINDRICAL_SURFACE('',#10234,0.991185);
#8325=CYLINDRICAL_SURFACE('',#10249,0.210000000000001);
#8326=CYLINDRICAL_SURFACE('',#10253,0.210000000000001);
#8327=CYLINDRICAL_SURFACE('',#10261,0.5);
#8328=CYLINDRICAL_SURFACE('',#10269,0.275);
#8329=CYLINDRICAL_SURFACE('',#10272,0.275);
#8330=CYLINDRICAL_SURFACE('',#10275,0.275);
#8331=CYLINDRICAL_SURFACE('',#10278,0.275);
#8332=CYLINDRICAL_SURFACE('',#10288,0.275);
#8333=CYLINDRICAL_SURFACE('',#10291,0.275);
#8334=CYLINDRICAL_SURFACE('',#10301,0.164999999999999);
#8335=CYLINDRICAL_SURFACE('',#10308,0.800000000000001);
#8336=CYLINDRICAL_SURFACE('',#10311,0.5);
#8337=CYLINDRICAL_SURFACE('',#10315,0.505000000000001);
#8338=CYLINDRICAL_SURFACE('',#10318,0.699999999999999);
#8339=CYLINDRICAL_SURFACE('',#10324,0.505000000000001);
#8340=CYLINDRICAL_SURFACE('',#10327,0.699999999999999);
#8341=CYLINDRICAL_SURFACE('',#10333,0.225);
#8342=CYLINDRICAL_SURFACE('',#10336,0.800000000000001);
#8343=CYLINDRICAL_SURFACE('',#10345,0.21);
#8344=CYLINDRICAL_SURFACE('',#10351,0.21);
#8345=CYLINDRICAL_SURFACE('',#10357,0.21);
#8346=CYLINDRICAL_SURFACE('',#10363,0.21);
#8347=CYLINDRICAL_SURFACE('',#10421,0.425);
#8348=CYLINDRICAL_SURFACE('',#10429,0.24505);
#8349=CYLINDRICAL_SURFACE('',#10434,0.265);
#8350=CYLINDRICAL_SURFACE('',#10438,0.5);
#8351=CYLINDRICAL_SURFACE('',#10446,0.425);
#8352=CYLINDRICAL_SURFACE('',#10454,0.24505);
#8353=CYLINDRICAL_SURFACE('',#10519,0.35);
#8354=CYLINDRICAL_SURFACE('',#10527,0.1954);
#8355=ADVANCED_FACE('',(#1217),#8196,.F.);
#8356=ADVANCED_FACE('',(#1218),#8197,.F.);
#8357=ADVANCED_FACE('',(#1219),#8198,.F.);
#8358=ADVANCED_FACE('',(#1220),#8199,.F.);
#8359=ADVANCED_FACE('',(#1221),#8200,.F.);
#8360=ADVANCED_FACE('',(#1222),#8201,.F.);
#8361=ADVANCED_FACE('',(#1223),#8202,.F.);
#8362=ADVANCED_FACE('',(#1224),#8203,.F.);
#8363=ADVANCED_FACE('',(#1225),#8204,.F.);
#8364=ADVANCED_FACE('',(#1226),#8205,.F.);
#8365=ADVANCED_FACE('',(#1227),#8206,.F.);
#8366=ADVANCED_FACE('',(#1228),#8207,.F.);
#8367=ADVANCED_FACE('',(#1229),#897,.T.);
#8368=ADVANCED_FACE('',(#1230),#898,.T.);
#8369=ADVANCED_FACE('',(#1231),#899,.T.);
#8370=ADVANCED_FACE('',(#1232),#900,.T.);
#8371=ADVANCED_FACE('',(#1233,#700,#701,#702,#703,#704,#705,#706,#707,#708,
#709,#710,#711),#901,.T.);
#8372=ADVANCED_FACE('',(#1234,#712,#713,#714,#715,#716,#717,#718,#719,#720,
#721,#722,#723),#902,.F.);
#8373=ADVANCED_FACE('',(#1235),#8208,.F.);
#8374=ADVANCED_FACE('',(#1236),#903,.T.);
#8375=ADVANCED_FACE('',(#1237),#8209,.F.);
#8376=ADVANCED_FACE('',(#1238),#904,.T.);
#8377=ADVANCED_FACE('',(#1239),#8210,.F.);
#8378=ADVANCED_FACE('',(#1240,#724),#905,.T.);
#8379=ADVANCED_FACE('',(#1241),#8211,.F.);
#8380=ADVANCED_FACE('',(#1242,#725),#906,.T.);
#8381=ADVANCED_FACE('',(#1243),#8212,.F.);
#8382=ADVANCED_FACE('',(#1244,#726),#907,.T.);
#8383=ADVANCED_FACE('',(#1245),#8213,.F.);
#8384=ADVANCED_FACE('',(#1246,#727),#908,.T.);
#8385=ADVANCED_FACE('',(#1247),#8214,.F.);
#8386=ADVANCED_FACE('',(#1248),#8215,.F.);
#8387=ADVANCED_FACE('',(#1249),#8216,.F.);
#8388=ADVANCED_FACE('',(#1250),#8217,.F.);
#8389=ADVANCED_FACE('',(#1251),#909,.T.);
#8390=ADVANCED_FACE('',(#1252),#910,.T.);
#8391=ADVANCED_FACE('',(#1253),#911,.T.);
#8392=ADVANCED_FACE('',(#1254),#912,.T.);
#8393=ADVANCED_FACE('',(#1255,#728,#729,#730,#731,#732,#733),#913,.T.);
#8394=ADVANCED_FACE('',(#1256,#734,#735,#736,#737),#914,.F.);
#8395=ADVANCED_FACE('',(#1257),#8218,.F.);
#8396=ADVANCED_FACE('',(#1258),#8219,.T.);
#8397=ADVANCED_FACE('',(#1259,#738),#915,.T.);
#8398=ADVANCED_FACE('',(#1260,#739),#916,.F.);
#8399=ADVANCED_FACE('',(#1261),#8220,.F.);
#8400=ADVANCED_FACE('',(#1262),#8221,.T.);
#8401=ADVANCED_FACE('',(#1263,#740),#917,.T.);
#8402=ADVANCED_FACE('',(#1264,#741),#918,.F.);
#8403=ADVANCED_FACE('',(#1265),#8222,.F.);
#8404=ADVANCED_FACE('',(#1266),#919,.T.);
#8405=ADVANCED_FACE('',(#1267),#8223,.F.);
#8406=ADVANCED_FACE('',(#1268),#920,.T.);
#8407=ADVANCED_FACE('',(#1269),#8224,.F.);
#8408=ADVANCED_FACE('',(#1270,#742),#921,.T.);
#8409=ADVANCED_FACE('',(#1271),#8225,.F.);
#8410=ADVANCED_FACE('',(#1272,#743),#922,.T.);
#8411=ADVANCED_FACE('',(#1273),#8226,.F.);
#8412=ADVANCED_FACE('',(#1274,#744),#923,.T.);
#8413=ADVANCED_FACE('',(#1275),#8227,.F.);
#8414=ADVANCED_FACE('',(#1276,#745),#924,.T.);
#8415=ADVANCED_FACE('',(#1277),#8228,.F.);
#8416=ADVANCED_FACE('',(#1278),#8229,.F.);
#8417=ADVANCED_FACE('',(#1279),#8230,.F.);
#8418=ADVANCED_FACE('',(#1280),#8231,.F.);
#8419=ADVANCED_FACE('',(#1281),#925,.T.);
#8420=ADVANCED_FACE('',(#1282),#926,.T.);
#8421=ADVANCED_FACE('',(#1283),#927,.T.);
#8422=ADVANCED_FACE('',(#1284),#928,.T.);
#8423=ADVANCED_FACE('',(#1285,#746,#747,#748,#749,#750,#751),#929,.T.);
#8424=ADVANCED_FACE('',(#1286,#752,#753,#754,#755),#930,.F.);
#8425=ADVANCED_FACE('',(#1287),#8232,.F.);
#8426=ADVANCED_FACE('',(#1288),#8233,.T.);
#8427=ADVANCED_FACE('',(#1289,#756),#931,.T.);
#8428=ADVANCED_FACE('',(#1290,#757),#932,.F.);
#8429=ADVANCED_FACE('',(#1291),#8234,.F.);
#8430=ADVANCED_FACE('',(#1292),#8235,.T.);
#8431=ADVANCED_FACE('',(#1293,#758),#933,.T.);
#8432=ADVANCED_FACE('',(#1294,#759),#934,.F.);
#8433=ADVANCED_FACE('',(#1295),#8236,.F.);
#8434=ADVANCED_FACE('',(#1296),#935,.T.);
#8435=ADVANCED_FACE('',(#1297),#8237,.F.);
#8436=ADVANCED_FACE('',(#1298),#936,.T.);
#8437=ADVANCED_FACE('',(#1299),#8238,.F.);
#8438=ADVANCED_FACE('',(#1300),#937,.T.);
#8439=ADVANCED_FACE('',(#1301),#8239,.F.);
#8440=ADVANCED_FACE('',(#1302),#938,.T.);
#8441=ADVANCED_FACE('',(#1303),#8240,.F.);
#8442=ADVANCED_FACE('',(#1304,#760),#939,.T.);
#8443=ADVANCED_FACE('',(#1305),#8241,.F.);
#8444=ADVANCED_FACE('',(#1306,#761),#940,.T.);
#8445=ADVANCED_FACE('',(#1307),#8242,.F.);
#8446=ADVANCED_FACE('',(#1308,#762),#941,.T.);
#8447=ADVANCED_FACE('',(#1309),#8243,.F.);
#8448=ADVANCED_FACE('',(#1310,#763),#942,.T.);
#8449=ADVANCED_FACE('',(#1311),#8244,.F.);
#8450=ADVANCED_FACE('',(#1312),#8245,.F.);
#8451=ADVANCED_FACE('',(#1313),#8246,.F.);
#8452=ADVANCED_FACE('',(#1314),#8247,.F.);
#8453=ADVANCED_FACE('',(#1315),#943,.T.);
#8454=ADVANCED_FACE('',(#1316),#944,.T.);
#8455=ADVANCED_FACE('',(#1317),#945,.T.);
#8456=ADVANCED_FACE('',(#1318),#946,.T.);
#8457=ADVANCED_FACE('',(#1319,#764,#765,#766,#767,#768,#769,#770,#771),
#947,.T.);
#8458=ADVANCED_FACE('',(#1320,#772,#773,#774,#775),#948,.F.);
#8459=ADVANCED_FACE('',(#1321),#949,.T.);
#8460=ADVANCED_FACE('',(#1322),#950,.T.);
#8461=ADVANCED_FACE('',(#1323),#951,.T.);
#8462=ADVANCED_FACE('',(#1324),#952,.T.);
#8463=ADVANCED_FACE('',(#1325),#953,.T.);
#8464=ADVANCED_FACE('',(#1326),#954,.F.);
#8465=ADVANCED_FACE('',(#1327),#955,.T.);
#8466=ADVANCED_FACE('',(#1328),#956,.T.);
#8467=ADVANCED_FACE('',(#1329),#957,.T.);
#8468=ADVANCED_FACE('',(#1330),#958,.T.);
#8469=ADVANCED_FACE('',(#1331),#959,.T.);
#8470=ADVANCED_FACE('',(#1332),#960,.F.);
#8471=ADVANCED_FACE('',(#1333),#8248,.F.);
#8472=ADVANCED_FACE('',(#1334),#8249,.F.);
#8473=ADVANCED_FACE('',(#1335,#776,#777),#469,.F.);
#8474=ADVANCED_FACE('',(#1336),#961,.T.);
#8475=ADVANCED_FACE('',(#1337),#962,.T.);
#8476=ADVANCED_FACE('',(#1338),#963,.T.);
#8477=ADVANCED_FACE('',(#1339),#964,.T.);
#8478=ADVANCED_FACE('',(#1340),#965,.T.);
#8479=ADVANCED_FACE('',(#1341),#966,.T.);
#8480=ADVANCED_FACE('',(#1342,#778,#779,#780),#967,.T.);
#8481=ADVANCED_FACE('',(#1343),#8250,.T.);
#8482=ADVANCED_FACE('',(#1344,#781),#968,.F.);
#8483=ADVANCED_FACE('',(#1345,#782),#969,.T.);
#8484=ADVANCED_FACE('',(#1346),#970,.F.);
#8485=ADVANCED_FACE('',(#1347),#971,.F.);
#8486=ADVANCED_FACE('',(#1348),#972,.F.);
#8487=ADVANCED_FACE('',(#1349),#973,.F.);
#8488=ADVANCED_FACE('',(#1350),#974,.F.);
#8489=ADVANCED_FACE('',(#1351),#8251,.F.);
#8490=ADVANCED_FACE('',(#1352),#8252,.F.);
#8491=ADVANCED_FACE('',(#1353),#975,.T.);
#8492=ADVANCED_FACE('',(#1354),#976,.T.);
#8493=ADVANCED_FACE('',(#1355),#977,.T.);
#8494=ADVANCED_FACE('',(#1356),#978,.T.);
#8495=ADVANCED_FACE('',(#1357,#783,#784,#785),#979,.F.);
#8496=ADVANCED_FACE('',(#1358),#8253,.F.);
#8497=ADVANCED_FACE('',(#1359,#786),#980,.T.);
#8498=ADVANCED_FACE('',(#1360,#787,#788),#470,.T.);
#8499=ADVANCED_FACE('',(#1361,#789),#981,.T.);
#8500=ADVANCED_FACE('',(#1362),#8254,.F.);
#8501=ADVANCED_FACE('',(#1363),#8255,.F.);
#8502=ADVANCED_FACE('',(#1364,#790,#791,#792,#793,#794,#795),#8256,.T.);
#8503=ADVANCED_FACE('',(#1365),#8257,.F.);
#8504=ADVANCED_FACE('',(#1366),#8258,.F.);
#8505=ADVANCED_FACE('',(#1367),#8259,.F.);
#8506=ADVANCED_FACE('',(#1368),#8260,.F.);
#8507=ADVANCED_FACE('',(#1369,#796),#982,.T.);
#8508=ADVANCED_FACE('',(#1370,#797),#983,.T.);
#8509=ADVANCED_FACE('',(#1371),#8261,.T.);
#8510=ADVANCED_FACE('',(#1372,#798),#984,.T.);
#8511=ADVANCED_FACE('',(#1373,#799,#800,#801,#802,#803,#804),#8262,.F.);
#8512=ADVANCED_FACE('',(#1374),#8263,.F.);
#8513=ADVANCED_FACE('',(#1375),#8264,.T.);
#8514=ADVANCED_FACE('',(#1376,#805),#985,.T.);
#8515=ADVANCED_FACE('',(#1377,#806),#986,.F.);
#8516=ADVANCED_FACE('',(#1378),#987,.F.);
#8517=ADVANCED_FACE('',(#1379),#988,.F.);
#8518=ADVANCED_FACE('',(#1380),#989,.F.);
#8519=ADVANCED_FACE('',(#1381),#990,.F.);
#8520=ADVANCED_FACE('',(#1382),#991,.F.);
#8521=ADVANCED_FACE('',(#1383),#992,.F.);
#8522=ADVANCED_FACE('',(#1384),#993,.F.);
#8523=ADVANCED_FACE('',(#1385),#994,.F.);
#8524=ADVANCED_FACE('',(#1386),#995,.F.);
#8525=ADVANCED_FACE('',(#1387),#996,.T.);
#8526=ADVANCED_FACE('',(#1388),#13,.T.);
#8527=ADVANCED_FACE('',(#1389),#8265,.T.);
#8528=ADVANCED_FACE('',(#1390),#14,.T.);
#8529=ADVANCED_FACE('',(#1391,#807),#997,.T.);
#8530=ADVANCED_FACE('',(#1392),#15,.T.);
#8531=ADVANCED_FACE('',(#1393),#8266,.T.);
#8532=ADVANCED_FACE('',(#1394),#8267,.F.);
#8533=ADVANCED_FACE('',(#1395,#808),#998,.T.);
#8534=ADVANCED_FACE('',(#1396),#8268,.F.);
#8535=ADVANCED_FACE('',(#1397,#809),#999,.T.);
#8536=ADVANCED_FACE('',(#1398),#8269,.F.);
#8537=ADVANCED_FACE('',(#1399,#810),#1000,.T.);
#8538=ADVANCED_FACE('',(#1400),#8270,.F.);
#8539=ADVANCED_FACE('',(#1401,#811),#1001,.T.);
#8540=ADVANCED_FACE('',(#1402),#8271,.F.);
#8541=ADVANCED_FACE('',(#1403),#8272,.F.);
#8542=ADVANCED_FACE('',(#1404),#8273,.F.);
#8543=ADVANCED_FACE('',(#1405),#8274,.F.);
#8544=ADVANCED_FACE('',(#1406),#1002,.T.);
#8545=ADVANCED_FACE('',(#1407),#1003,.T.);
#8546=ADVANCED_FACE('',(#1408),#1004,.T.);
#8547=ADVANCED_FACE('',(#1409),#1005,.T.);
#8548=ADVANCED_FACE('',(#1410,#812,#813,#814,#815),#1006,.T.);
#8549=ADVANCED_FACE('',(#1411),#1007,.T.);
#8550=ADVANCED_FACE('',(#1412),#1008,.T.);
#8551=ADVANCED_FACE('',(#1413),#1009,.T.);
#8552=ADVANCED_FACE('',(#1414),#1010,.T.);
#8553=ADVANCED_FACE('',(#1415),#1011,.T.);
#8554=ADVANCED_FACE('',(#1416,#816,#817,#818,#819),#1012,.T.);
#8555=ADVANCED_FACE('',(#1417),#1013,.T.);
#8556=ADVANCED_FACE('',(#1418),#1014,.T.);
#8557=ADVANCED_FACE('',(#1419),#1015,.F.);
#8558=ADVANCED_FACE('',(#1420),#1016,.T.);
#8559=ADVANCED_FACE('',(#1421),#16,.T.);
#8560=ADVANCED_FACE('',(#1422),#8275,.T.);
#8561=ADVANCED_FACE('',(#1423),#17,.T.);
#8562=ADVANCED_FACE('',(#1424,#820),#1017,.T.);
#8563=ADVANCED_FACE('',(#1425),#18,.T.);
#8564=ADVANCED_FACE('',(#1426),#8276,.T.);
#8565=ADVANCED_FACE('',(#1427),#19,.T.);
#8566=ADVANCED_FACE('',(#1428),#1018,.T.);
#8567=ADVANCED_FACE('',(#1429),#1019,.F.);
#8568=ADVANCED_FACE('',(#1430),#1020,.F.);
#8569=ADVANCED_FACE('',(#1431),#1021,.F.);
#8570=ADVANCED_FACE('',(#1432),#1022,.F.);
#8571=ADVANCED_FACE('',(#1433),#1023,.F.);
#8572=ADVANCED_FACE('',(#1434),#1024,.F.);
#8573=ADVANCED_FACE('',(#1435),#1025,.F.);
#8574=ADVANCED_FACE('',(#1436),#1026,.F.);
#8575=ADVANCED_FACE('',(#1437),#1027,.F.);
#8576=ADVANCED_FACE('',(#1438),#1028,.T.);
#8577=ADVANCED_FACE('',(#1439),#1029,.F.);
#8578=ADVANCED_FACE('',(#1440),#1030,.F.);
#8579=ADVANCED_FACE('',(#1441),#8277,.T.);
#8580=ADVANCED_FACE('',(#1442),#1031,.T.);
#8581=ADVANCED_FACE('',(#1443),#1032,.F.);
#8582=ADVANCED_FACE('',(#1444),#1033,.T.);
#8583=ADVANCED_FACE('',(#1445),#8278,.F.);
#8584=ADVANCED_FACE('',(#1446),#1034,.T.);
#8585=ADVANCED_FACE('',(#1447,#821),#8279,.F.);
#8586=ADVANCED_FACE('',(#1448,#822),#8280,.T.);
#8587=ADVANCED_FACE('',(#1449,#823),#1035,.T.);
#8588=ADVANCED_FACE('',(#1450,#824),#1036,.F.);
#8589=ADVANCED_FACE('',(#1451),#1037,.T.);
#8590=ADVANCED_FACE('',(#1452),#8281,.F.);
#8591=ADVANCED_FACE('',(#1453),#1038,.T.);
#8592=ADVANCED_FACE('',(#1454,#825),#8282,.F.);
#8593=ADVANCED_FACE('',(#1455,#826),#8283,.T.);
#8594=ADVANCED_FACE('',(#1456,#827),#1039,.T.);
#8595=ADVANCED_FACE('',(#1457,#828),#1040,.F.);
#8596=ADVANCED_FACE('',(#1458),#8284,.F.);
#8597=ADVANCED_FACE('',(#1459),#8285,.T.);
#8598=ADVANCED_FACE('',(#1460,#829),#1041,.T.);
#8599=ADVANCED_FACE('',(#1461,#830),#1042,.F.);
#8600=ADVANCED_FACE('',(#1462),#1043,.T.);
#8601=ADVANCED_FACE('',(#1463),#8286,.F.);
#8602=ADVANCED_FACE('',(#1464),#8287,.F.);
#8603=ADVANCED_FACE('',(#1465),#1044,.F.);
#8604=ADVANCED_FACE('',(#1466,#831),#1045,.T.);
#8605=ADVANCED_FACE('',(#1467),#1046,.F.);
#8606=ADVANCED_FACE('',(#1468),#1047,.F.);
#8607=ADVANCED_FACE('',(#1469),#1048,.T.);
#8608=ADVANCED_FACE('',(#1470),#8288,.F.);
#8609=ADVANCED_FACE('',(#1471),#1049,.T.);
#8610=ADVANCED_FACE('',(#1472),#1050,.F.);
#8611=ADVANCED_FACE('',(#1473,#832),#1051,.F.);
#8612=ADVANCED_FACE('',(#1474),#8289,.T.);
#8613=ADVANCED_FACE('',(#1475),#8290,.T.);
#8614=ADVANCED_FACE('',(#1476),#1052,.F.);
#8615=ADVANCED_FACE('',(#1477),#8291,.F.);
#8616=ADVANCED_FACE('',(#1478),#1053,.T.);
#8617=ADVANCED_FACE('',(#1479,#833),#1054,.F.);
#8618=ADVANCED_FACE('',(#1480),#8292,.T.);
#8619=ADVANCED_FACE('',(#1481,#834),#1055,.T.);
#8620=ADVANCED_FACE('',(#1482),#8293,.T.);
#8621=ADVANCED_FACE('',(#1483),#1056,.F.);
#8622=ADVANCED_FACE('',(#1484),#8294,.F.);
#8623=ADVANCED_FACE('',(#1485),#8295,.T.);
#8624=ADVANCED_FACE('',(#1486,#835),#1057,.T.);
#8625=ADVANCED_FACE('',(#1487,#836),#1058,.F.);
#8626=ADVANCED_FACE('',(#1488),#8296,.F.);
#8627=ADVANCED_FACE('',(#1489),#8297,.T.);
#8628=ADVANCED_FACE('',(#1490,#837),#1059,.T.);
#8629=ADVANCED_FACE('',(#1491,#838),#1060,.F.);
#8630=ADVANCED_FACE('',(#1492),#8298,.F.);
#8631=ADVANCED_FACE('',(#1493),#8299,.T.);
#8632=ADVANCED_FACE('',(#1494,#839),#1061,.T.);
#8633=ADVANCED_FACE('',(#1495,#840),#1062,.F.);
#8634=ADVANCED_FACE('',(#1496),#1063,.F.);
#8635=ADVANCED_FACE('',(#1497),#1064,.T.);
#8636=ADVANCED_FACE('',(#1498),#1065,.T.);
#8637=ADVANCED_FACE('',(#1499),#1066,.T.);
#8638=ADVANCED_FACE('',(#1500),#1067,.T.);
#8639=ADVANCED_FACE('',(#1501),#1068,.T.);
#8640=ADVANCED_FACE('',(#1502),#1069,.F.);
#8641=ADVANCED_FACE('',(#1503),#1070,.T.);
#8642=ADVANCED_FACE('',(#1504),#1071,.T.);
#8643=ADVANCED_FACE('',(#1505),#1072,.T.);
#8644=ADVANCED_FACE('',(#1506),#1073,.F.);
#8645=ADVANCED_FACE('',(#1507),#1074,.F.);
#8646=ADVANCED_FACE('',(#1508),#1075,.F.);
#8647=ADVANCED_FACE('',(#1509),#1076,.F.);
#8648=ADVANCED_FACE('',(#1510),#1077,.F.);
#8649=ADVANCED_FACE('',(#1511),#1078,.F.);
#8650=ADVANCED_FACE('',(#1512),#1079,.F.);
#8651=ADVANCED_FACE('',(#1513,#841),#1080,.T.);
#8652=ADVANCED_FACE('',(#1514),#20,.T.);
#8653=ADVANCED_FACE('',(#1515),#8300,.T.);
#8654=ADVANCED_FACE('',(#1516),#21,.T.);
#8655=ADVANCED_FACE('',(#1517),#1081,.T.);
#8656=ADVANCED_FACE('',(#1518),#8301,.F.);
#8657=ADVANCED_FACE('',(#1519),#8302,.F.);
#8658=ADVANCED_FACE('',(#1520),#8303,.T.);
#8659=ADVANCED_FACE('',(#1521,#842,#843),#1082,.T.);
#8660=ADVANCED_FACE('',(#1522),#1083,.T.);
#8661=ADVANCED_FACE('',(#1523),#8304,.T.);
#8662=ADVANCED_FACE('',(#1524),#1084,.T.);
#8663=ADVANCED_FACE('',(#1525,#844,#845),#1085,.F.);
#8664=ADVANCED_FACE('',(#1526),#8305,.F.);
#8665=ADVANCED_FACE('',(#1527),#8306,.T.);
#8666=ADVANCED_FACE('',(#1528,#846),#1086,.T.);
#8667=ADVANCED_FACE('',(#1529,#847),#1087,.F.);
#8668=ADVANCED_FACE('',(#1530),#8307,.F.);
#8669=ADVANCED_FACE('',(#1531),#8308,.T.);
#8670=ADVANCED_FACE('',(#1532,#848),#1088,.T.);
#8671=ADVANCED_FACE('',(#1533,#849),#1089,.F.);
#8672=ADVANCED_FACE('',(#1534),#8309,.F.);
#8673=ADVANCED_FACE('',(#1535),#8310,.T.);
#8674=ADVANCED_FACE('',(#1536,#850),#1090,.T.);
#8675=ADVANCED_FACE('',(#1537,#851),#1091,.F.);
#8676=ADVANCED_FACE('',(#1538),#8311,.F.);
#8677=ADVANCED_FACE('',(#1539),#8312,.T.);
#8678=ADVANCED_FACE('',(#1540,#852),#1092,.T.);
#8679=ADVANCED_FACE('',(#1541,#853),#1093,.F.);
#8680=ADVANCED_FACE('',(#1542),#11,.F.);
#8681=ADVANCED_FACE('',(#1543),#8313,.T.);
#8682=ADVANCED_FACE('',(#1544),#8314,.F.);
#8683=ADVANCED_FACE('',(#1545),#22,.F.);
#8684=ADVANCED_FACE('',(#1546,#854),#1094,.T.);
#8685=ADVANCED_FACE('',(#1547),#8315,.T.);
#8686=ADVANCED_FACE('',(#1548,#855),#1095,.T.);
#8687=ADVANCED_FACE('',(#1549),#23,.F.);
#8688=ADVANCED_FACE('',(#1550),#12,.F.);
#8689=ADVANCED_FACE('',(#1551),#8316,.F.);
#8690=ADVANCED_FACE('',(#1552,#856),#1096,.T.);
#8691=ADVANCED_FACE('',(#1553),#24,.T.);
#8692=ADVANCED_FACE('',(#1554),#8317,.T.);
#8693=ADVANCED_FACE('',(#1555),#25,.T.);
#8694=ADVANCED_FACE('',(#1556,#857),#1097,.T.);
#8695=ADVANCED_FACE('',(#1557),#8318,.F.);
#8696=ADVANCED_FACE('',(#1558),#471,.T.);
#8697=ADVANCED_FACE('',(#1559),#472,.T.);
#8698=ADVANCED_FACE('',(#1560),#473,.T.);
#8699=ADVANCED_FACE('',(#1561),#474,.T.);
#8700=ADVANCED_FACE('',(#1562),#475,.T.);
#8701=ADVANCED_FACE('',(#1563),#476,.T.);
#8702=ADVANCED_FACE('',(#1564),#477,.T.);
#8703=ADVANCED_FACE('',(#1565),#478,.T.);
#8704=ADVANCED_FACE('',(#1566),#479,.F.);
#8705=ADVANCED_FACE('',(#1567),#8319,.T.);
#8706=ADVANCED_FACE('',(#1568),#1098,.T.);
#8707=ADVANCED_FACE('',(#1569),#480,.F.);
#8708=ADVANCED_FACE('',(#1570),#1099,.T.);
#8709=ADVANCED_FACE('',(#1571),#481,.F.);
#8710=ADVANCED_FACE('',(#1572),#1100,.T.);
#8711=ADVANCED_FACE('',(#1573),#482,.F.);
#8712=ADVANCED_FACE('',(#1574),#1101,.T.);
#8713=ADVANCED_FACE('',(#1575),#483,.F.);
#8714=ADVANCED_FACE('',(#1576),#1102,.T.);
#8715=ADVANCED_FACE('',(#1577),#484,.F.);
#8716=ADVANCED_FACE('',(#1578),#1103,.T.);
#8717=ADVANCED_FACE('',(#1579),#485,.F.);
#8718=ADVANCED_FACE('',(#1580),#8320,.F.);
#8719=ADVANCED_FACE('',(#1581),#1104,.T.);
#8720=ADVANCED_FACE('',(#1582),#486,.F.);
#8721=ADVANCED_FACE('',(#1583,#858),#1105,.T.);
#8722=ADVANCED_FACE('',(#1584),#1106,.T.);
#8723=ADVANCED_FACE('',(#1585,#859),#1107,.T.);
#8724=ADVANCED_FACE('',(#1586),#8321,.T.);
#8725=ADVANCED_FACE('',(#1587,#860),#1108,.T.);
#8726=ADVANCED_FACE('',(#1588),#8322,.F.);
#8727=ADVANCED_FACE('',(#1589,#861),#1109,.T.);
#8728=ADVANCED_FACE('',(#1590),#8323,.T.);
#8729=ADVANCED_FACE('',(#1591,#862),#1110,.T.);
#8730=ADVANCED_FACE('',(#1592),#8324,.F.);
#8731=ADVANCED_FACE('',(#1593),#8325,.F.);
#8732=ADVANCED_FACE('',(#1594),#1111,.T.);
#8733=ADVANCED_FACE('',(#1595),#8326,.F.);
#8734=ADVANCED_FACE('',(#1596),#1112,.T.);
#8735=ADVANCED_FACE('',(#1597),#1113,.T.);
#8736=ADVANCED_FACE('',(#1598),#1114,.T.);
#8737=ADVANCED_FACE('',(#1599,#863,#864),#1115,.T.);
#8738=ADVANCED_FACE('',(#1600),#1116,.T.);
#8739=ADVANCED_FACE('',(#1601),#8327,.F.);
#8740=ADVANCED_FACE('',(#1602,#865),#1117,.F.);
#8741=ADVANCED_FACE('',(#1603),#1118,.T.);
#8742=ADVANCED_FACE('',(#1604),#1119,.T.);
#8743=ADVANCED_FACE('',(#1605),#1120,.T.);
#8744=ADVANCED_FACE('',(#1606,#866),#1121,.T.);
#8745=ADVANCED_FACE('',(#1607),#8328,.F.);
#8746=ADVANCED_FACE('',(#1608),#8329,.F.);
#8747=ADVANCED_FACE('',(#1609),#8330,.F.);
#8748=ADVANCED_FACE('',(#1610),#8331,.F.);
#8749=ADVANCED_FACE('',(#1611),#1122,.T.);
#8750=ADVANCED_FACE('',(#1612),#1123,.T.);
#8751=ADVANCED_FACE('',(#1613),#1124,.T.);
#8752=ADVANCED_FACE('',(#1614),#1125,.T.);
#8753=ADVANCED_FACE('',(#1615,#867,#868,#869,#870,#871),#1126,.T.);
#8754=ADVANCED_FACE('',(#1616,#872,#873,#874,#875),#1127,.F.);
#8755=ADVANCED_FACE('',(#1617),#8332,.F.);
#8756=ADVANCED_FACE('',(#1618),#8333,.F.);
#8757=ADVANCED_FACE('',(#1619),#1128,.T.);
#8758=ADVANCED_FACE('',(#1620),#1129,.T.);
#8759=ADVANCED_FACE('',(#1621),#1130,.T.);
#8760=ADVANCED_FACE('',(#1622),#1131,.T.);
#8761=ADVANCED_FACE('',(#1623,#876,#877),#1132,.T.);
#8762=ADVANCED_FACE('',(#1624,#878,#879),#1133,.F.);
#8763=ADVANCED_FACE('',(#1625),#8334,.F.);
#8764=ADVANCED_FACE('',(#1626),#1134,.T.);
#8765=ADVANCED_FACE('',(#1627,#880),#1135,.T.);
#8766=ADVANCED_FACE('',(#1628),#8335,.T.);
#8767=ADVANCED_FACE('',(#1629),#1136,.F.);
#8768=ADVANCED_FACE('',(#1630),#8336,.T.);
#8769=ADVANCED_FACE('',(#1631,#881),#1137,.T.);
#8770=ADVANCED_FACE('',(#1632),#8337,.F.);
#8771=ADVANCED_FACE('',(#1633),#8338,.T.);
#8772=ADVANCED_FACE('',(#1634,#882),#1138,.T.);
#8773=ADVANCED_FACE('',(#1635,#883),#1139,.F.);
#8774=ADVANCED_FACE('',(#1636),#8339,.F.);
#8775=ADVANCED_FACE('',(#1637),#8340,.T.);
#8776=ADVANCED_FACE('',(#1638,#884),#1140,.T.);
#8777=ADVANCED_FACE('',(#1639,#885),#1141,.F.);
#8778=ADVANCED_FACE('',(#1640),#8341,.F.);
#8779=ADVANCED_FACE('',(#1641),#8342,.T.);
#8780=ADVANCED_FACE('',(#1642,#886),#1142,.T.);
#8781=ADVANCED_FACE('',(#1643,#887),#1143,.F.);
#8782=ADVANCED_FACE('',(#1644),#1144,.T.);
#8783=ADVANCED_FACE('',(#1645),#8343,.F.);
#8784=ADVANCED_FACE('',(#1646),#1145,.T.);
#8785=ADVANCED_FACE('',(#1647),#8344,.F.);
#8786=ADVANCED_FACE('',(#1648),#1146,.T.);
#8787=ADVANCED_FACE('',(#1649),#8345,.F.);
#8788=ADVANCED_FACE('',(#1650),#1147,.T.);
#8789=ADVANCED_FACE('',(#1651),#8346,.F.);
#8790=ADVANCED_FACE('',(#1652),#1148,.T.);
#8791=ADVANCED_FACE('',(#1653),#1149,.T.);
#8792=ADVANCED_FACE('',(#1654),#1150,.T.);
#8793=ADVANCED_FACE('',(#1655),#1151,.T.);
#8794=ADVANCED_FACE('',(#1656),#1152,.T.);
#8795=ADVANCED_FACE('',(#1657,#888,#889,#890,#891),#1153,.T.);
#8796=ADVANCED_FACE('',(#1658),#1154,.T.);
#8797=ADVANCED_FACE('',(#1659),#1155,.T.);
#8798=ADVANCED_FACE('',(#1660),#1156,.T.);
#8799=ADVANCED_FACE('',(#1661),#1157,.T.);
#8800=ADVANCED_FACE('',(#1662),#1158,.T.);
#8801=ADVANCED_FACE('',(#1663),#1159,.T.);
#8802=ADVANCED_FACE('',(#1664),#1160,.T.);
#8803=ADVANCED_FACE('',(#1665),#1161,.T.);
#8804=ADVANCED_FACE('',(#1666),#1162,.T.);
#8805=ADVANCED_FACE('',(#1667),#1163,.T.);
#8806=ADVANCED_FACE('',(#1668),#1164,.T.);
#8807=ADVANCED_FACE('',(#1669),#1165,.T.);
#8808=ADVANCED_FACE('',(#1670),#1166,.T.);
#8809=ADVANCED_FACE('',(#1671),#1167,.T.);
#8810=ADVANCED_FACE('',(#1672),#1168,.T.);
#8811=ADVANCED_FACE('',(#1673),#1169,.T.);
#8812=ADVANCED_FACE('',(#1674),#1170,.T.);
#8813=ADVANCED_FACE('',(#1675),#1171,.F.);
#8814=ADVANCED_FACE('',(#1676),#1172,.T.);
#8815=ADVANCED_FACE('',(#1677),#1173,.T.);
#8816=ADVANCED_FACE('',(#1678),#1174,.T.);
#8817=ADVANCED_FACE('',(#1679),#1175,.T.);
#8818=ADVANCED_FACE('',(#1680),#1176,.T.);
#8819=ADVANCED_FACE('',(#1681),#1177,.T.);
#8820=ADVANCED_FACE('',(#1682),#1178,.T.);
#8821=ADVANCED_FACE('',(#1683),#1179,.T.);
#8822=ADVANCED_FACE('',(#1684),#1180,.T.);
#8823=ADVANCED_FACE('',(#1685),#1181,.T.);
#8824=ADVANCED_FACE('',(#1686),#1182,.F.);
#8825=ADVANCED_FACE('',(#1687),#1183,.F.);
#8826=ADVANCED_FACE('',(#1688),#1184,.F.);
#8827=ADVANCED_FACE('',(#1689),#1185,.F.);
#8828=ADVANCED_FACE('',(#1690),#1186,.F.);
#8829=ADVANCED_FACE('',(#1691),#1187,.F.);
#8830=ADVANCED_FACE('',(#1692),#1188,.F.);
#8831=ADVANCED_FACE('',(#1693),#1189,.F.);
#8832=ADVANCED_FACE('',(#1694),#1190,.F.);
#8833=ADVANCED_FACE('',(#1695),#1191,.T.);
#8834=ADVANCED_FACE('',(#1696),#26,.T.);
#8835=ADVANCED_FACE('',(#1697),#8347,.T.);
#8836=ADVANCED_FACE('',(#1698),#27,.T.);
#8837=ADVANCED_FACE('',(#1699,#892),#1192,.T.);
#8838=ADVANCED_FACE('',(#1700),#28,.T.);
#8839=ADVANCED_FACE('',(#1701),#8348,.T.);
#8840=ADVANCED_FACE('',(#1702),#29,.F.);
#8841=ADVANCED_FACE('',(#1703),#8349,.F.);
#8842=ADVANCED_FACE('',(#1704,#893),#1193,.T.);
#8843=ADVANCED_FACE('',(#1705),#8350,.T.);
#8844=ADVANCED_FACE('',(#1706,#894),#1194,.F.);
#8845=ADVANCED_FACE('',(#1707),#1195,.T.);
#8846=ADVANCED_FACE('',(#1708),#30,.T.);
#8847=ADVANCED_FACE('',(#1709),#8351,.T.);
#8848=ADVANCED_FACE('',(#1710),#31,.T.);
#8849=ADVANCED_FACE('',(#1711,#895),#1196,.T.);
#8850=ADVANCED_FACE('',(#1712),#32,.T.);
#8851=ADVANCED_FACE('',(#1713),#8352,.T.);
#8852=ADVANCED_FACE('',(#1714),#33,.T.);
#8853=ADVANCED_FACE('',(#1715),#1197,.T.);
#8854=ADVANCED_FACE('',(#1716),#1198,.F.);
#8855=ADVANCED_FACE('',(#1717),#1199,.F.);
#8856=ADVANCED_FACE('',(#1718),#1200,.F.);
#8857=ADVANCED_FACE('',(#1719),#1201,.F.);
#8858=ADVANCED_FACE('',(#1720),#1202,.F.);
#8859=ADVANCED_FACE('',(#1721),#1203,.F.);
#8860=ADVANCED_FACE('',(#1722),#1204,.F.);
#8861=ADVANCED_FACE('',(#1723),#1205,.F.);
#8862=ADVANCED_FACE('',(#1724),#1206,.F.);
#8863=ADVANCED_FACE('',(#1725),#1207,.F.);
#8864=ADVANCED_FACE('',(#1726),#1208,.F.);
#8865=ADVANCED_FACE('',(#1727),#1209,.F.);
#8866=ADVANCED_FACE('',(#1728),#1210,.F.);
#8867=ADVANCED_FACE('',(#1729),#1211,.F.);
#8868=ADVANCED_FACE('',(#1730),#1212,.F.);
#8869=ADVANCED_FACE('',(#1731),#1213,.F.);
#8870=ADVANCED_FACE('',(#1732),#1214,.F.);
#8871=ADVANCED_FACE('',(#1733),#1215,.T.);
#8872=ADVANCED_FACE('',(#1734),#34,.T.);
#8873=ADVANCED_FACE('',(#1735),#8353,.T.);
#8874=ADVANCED_FACE('',(#1736),#35,.T.);
#8875=ADVANCED_FACE('',(#1737,#896),#1216,.T.);
#8876=ADVANCED_FACE('',(#1738),#36,.T.);
#8877=ADVANCED_FACE('',(#1739),#8354,.T.);
#8878=CLOSED_SHELL('',(#8355,#8356,#8357,#8358,#8359,#8360,#8361,#8362,
#8363,#8364,#8365,#8366,#8367,#8368,#8369,#8370,#8371,#8372));
#8879=CLOSED_SHELL('',(#8373,#8374,#8375,#8376,#8377,#8378,#8379,#8380,
#8381,#8382,#8383,#8384,#8385,#8386,#8387,#8388,#8389,#8390,#8391,#8392,
#8393,#8394));
#8880=CLOSED_SHELL('',(#8395,#8396,#8397,#8398));
#8881=CLOSED_SHELL('',(#8399,#8400,#8401,#8402));
#8882=CLOSED_SHELL('',(#8403,#8404,#8405,#8406,#8407,#8408,#8409,#8410,
#8411,#8412,#8413,#8414,#8415,#8416,#8417,#8418,#8419,#8420,#8421,#8422,
#8423,#8424));
#8883=CLOSED_SHELL('',(#8425,#8426,#8427,#8428));
#8884=CLOSED_SHELL('',(#8429,#8430,#8431,#8432));
#8885=CLOSED_SHELL('',(#8433,#8434,#8435,#8436,#8437,#8438,#8439,#8440,
#8441,#8442,#8443,#8444,#8445,#8446,#8447,#8448,#8449,#8450,#8451,#8452,
#8453,#8454,#8455,#8456,#8457,#8458));
#8886=CLOSED_SHELL('',(#8459,#8460,#8461,#8462,#8463,#8464));
#8887=CLOSED_SHELL('',(#8465,#8466,#8467,#8468,#8469,#8470));
#8888=CLOSED_SHELL('',(#8471,#8472,#8473,#8474,#8475,#8476,#8477,#8478,
#8479,#8480,#8481,#8482,#8483,#8484,#8485,#8486,#8487,#8488,#8489,#8490,
#8491,#8492,#8493,#8494,#8495));
#8889=CLOSED_SHELL('',(#8496,#8497,#8498,#8499));
#8890=CLOSED_SHELL('',(#8500,#8501,#8502,#8503,#8504,#8505,#8506,#8507,
#8508,#8509,#8510,#8511));
#8891=CLOSED_SHELL('',(#8512,#8513,#8514,#8515));
#8892=CLOSED_SHELL('',(#8516,#8517,#8518,#8519,#8520,#8521,#8522,#8523));
#8893=CLOSED_SHELL('',(#8524,#8525,#8526,#8527,#8528,#8529,#8530,#8531));
#8894=CLOSED_SHELL('',(#8532,#8533,#8534,#8535,#8536,#8537,#8538,#8539,
#8540,#8541,#8542,#8543,#8544,#8545,#8546,#8547,#8548,#8549,#8550,#8551,
#8552,#8553,#8554,#8555,#8556,#8557));
#8895=CLOSED_SHELL('',(#8558,#8559,#8560,#8561,#8562,#8563,#8564,#8565,
#8566));
#8896=CLOSED_SHELL('',(#8567,#8568,#8569,#8570,#8571,#8572,#8573,#8574));
#8897=CLOSED_SHELL('',(#8575,#8576,#8577,#8578,#8579,#8580,#8581));
#8898=CLOSED_SHELL('',(#8582,#8583,#8584,#8585,#8586,#8587,#8588));
#8899=CLOSED_SHELL('',(#8589,#8590,#8591,#8592,#8593,#8594,#8595));
#8900=CLOSED_SHELL('',(#8596,#8597,#8598,#8599));
#8901=CLOSED_SHELL('',(#8600,#8601,#8602,#8603,#8604,#8605,#8606,#8607,
#8608,#8609,#8610,#8611,#8612,#8613,#8614));
#8902=CLOSED_SHELL('',(#8615,#8616,#8617,#8618,#8619,#8620,#8621));
#8903=CLOSED_SHELL('',(#8622,#8623,#8624,#8625));
#8904=CLOSED_SHELL('',(#8626,#8627,#8628,#8629));
#8905=CLOSED_SHELL('',(#8630,#8631,#8632,#8633));
#8906=CLOSED_SHELL('',(#8634,#8635,#8636,#8637,#8638,#8639,#8640,#8641,
#8642,#8643));
#8907=CLOSED_SHELL('',(#8644,#8645,#8646,#8647,#8648,#8649,#8650,#8651,
#8652,#8653,#8654,#8655));
#8908=CLOSED_SHELL('',(#8656,#8657,#8658,#8659,#8660,#8661,#8662,#8663));
#8909=CLOSED_SHELL('',(#8664,#8665,#8666,#8667));
#8910=CLOSED_SHELL('',(#8668,#8669,#8670,#8671));
#8911=CLOSED_SHELL('',(#8672,#8673,#8674,#8675));
#8912=CLOSED_SHELL('',(#8676,#8677,#8678,#8679));
#8913=CLOSED_SHELL('',(#8680,#8681,#8682,#8683,#8684,#8685,#8686,#8687));
#8914=CLOSED_SHELL('',(#8688,#8689,#8690,#8691,#8692,#8693,#8694,#8695));
#8915=CLOSED_SHELL('',(#8696));
#8916=CLOSED_SHELL('',(#8697));
#8917=CLOSED_SHELL('',(#8698));
#8918=CLOSED_SHELL('',(#8699));
#8919=CLOSED_SHELL('',(#8700));
#8920=CLOSED_SHELL('',(#8701));
#8921=CLOSED_SHELL('',(#8702));
#8922=CLOSED_SHELL('',(#8703));
#8923=CLOSED_SHELL('',(#8704,#8705,#8706,#8707,#8708,#8709,#8710,#8711,
#8712,#8713,#8714,#8715,#8716,#8717,#8718,#8719,#8720,#8721,#8722));
#8924=CLOSED_SHELL('',(#8723,#8724,#8725,#8726));
#8925=CLOSED_SHELL('',(#8727,#8728,#8729,#8730));
#8926=CLOSED_SHELL('',(#8731,#8732,#8733,#8734,#8735,#8736,#8737,#8738,
#8739,#8740,#8741,#8742,#8743,#8744,#8745,#8746,#8747,#8748,#8749,#8750,
#8751,#8752,#8753,#8754));
#8927=CLOSED_SHELL('',(#8755,#8756,#8757,#8758,#8759,#8760,#8761,#8762));
#8928=CLOSED_SHELL('',(#8763,#8764,#8765,#8766,#8767,#8768,#8769));
#8929=CLOSED_SHELL('',(#8770,#8771,#8772,#8773));
#8930=CLOSED_SHELL('',(#8774,#8775,#8776,#8777));
#8931=CLOSED_SHELL('',(#8778,#8779,#8780,#8781));
#8932=CLOSED_SHELL('',(#8782,#8783,#8784,#8785,#8786,#8787,#8788,#8789,
#8790,#8791,#8792,#8793,#8794,#8795,#8796,#8797,#8798,#8799,#8800,#8801,
#8802,#8803));
#8933=CLOSED_SHELL('',(#8804,#8805,#8806,#8807,#8808,#8809,#8810,#8811,
#8812,#8813));
#8934=CLOSED_SHELL('',(#8814,#8815,#8816,#8817,#8818,#8819,#8820,#8821,
#8822,#8823));
#8935=CLOSED_SHELL('',(#8824,#8825,#8826,#8827,#8828,#8829,#8830,#8831));
#8936=CLOSED_SHELL('',(#8832,#8833,#8834,#8835,#8836,#8837,#8838,#8839));
#8937=CLOSED_SHELL('',(#8840,#8841,#8842,#8843,#8844));
#8938=CLOSED_SHELL('',(#8845,#8846,#8847,#8848,#8849,#8850,#8851,#8852,
#8853));
#8939=CLOSED_SHELL('',(#8854,#8855,#8856,#8857,#8858,#8859,#8860,#8861));
#8940=CLOSED_SHELL('',(#8862,#8863,#8864,#8865,#8866,#8867,#8868,#8869));
#8941=CLOSED_SHELL('',(#8870,#8871,#8872,#8873,#8874,#8875,#8876,#8877));
#8942=DERIVED_UNIT_ELEMENT(#9042,1.);
#8943=DERIVED_UNIT_ELEMENT(#16913,-3.);
#8944=DERIVED_UNIT_ELEMENT(#9042,1.);
#8945=DERIVED_UNIT_ELEMENT(#16913,-3.);
#8946=DERIVED_UNIT_ELEMENT(#9042,1.);
#8947=DERIVED_UNIT_ELEMENT(#16913,-3.);
#8948=DERIVED_UNIT_ELEMENT(#9042,1.);
#8949=DERIVED_UNIT_ELEMENT(#16913,-3.);
#8950=DERIVED_UNIT_ELEMENT(#9042,1.);
#8951=DERIVED_UNIT_ELEMENT(#16913,-3.);
#8952=DERIVED_UNIT_ELEMENT(#9042,1.);
#8953=DERIVED_UNIT_ELEMENT(#16913,-3.);
#8954=DERIVED_UNIT_ELEMENT(#9042,1.);
#8955=DERIVED_UNIT_ELEMENT(#16913,-3.);
#8956=DERIVED_UNIT_ELEMENT(#9042,1.);
#8957=DERIVED_UNIT_ELEMENT(#16913,-3.);
#8958=DERIVED_UNIT_ELEMENT(#9042,1.);
#8959=DERIVED_UNIT_ELEMENT(#16913,-3.);
#8960=DERIVED_UNIT_ELEMENT(#9042,1.);
#8961=DERIVED_UNIT_ELEMENT(#16913,-3.);
#8962=DERIVED_UNIT_ELEMENT(#9042,1.);
#8963=DERIVED_UNIT_ELEMENT(#16913,-3.);
#8964=DERIVED_UNIT_ELEMENT(#9042,1.);
#8965=DERIVED_UNIT_ELEMENT(#16913,-3.);
#8966=DERIVED_UNIT_ELEMENT(#9042,1.);
#8967=DERIVED_UNIT_ELEMENT(#16913,-3.);
#8968=DERIVED_UNIT_ELEMENT(#9042,1.);
#8969=DERIVED_UNIT_ELEMENT(#16913,-3.);
#8970=DERIVED_UNIT_ELEMENT(#9042,1.);
#8971=DERIVED_UNIT_ELEMENT(#16913,-3.);
#8972=DERIVED_UNIT_ELEMENT(#9042,1.);
#8973=DERIVED_UNIT_ELEMENT(#16913,-3.);
#8974=DERIVED_UNIT_ELEMENT(#9042,1.);
#8975=DERIVED_UNIT_ELEMENT(#16913,-3.);
#8976=DERIVED_UNIT_ELEMENT(#9042,1.);
#8977=DERIVED_UNIT_ELEMENT(#16913,-3.);
#8978=DERIVED_UNIT_ELEMENT(#9042,1.);
#8979=DERIVED_UNIT_ELEMENT(#16913,-3.);
#8980=DERIVED_UNIT_ELEMENT(#9042,1.);
#8981=DERIVED_UNIT_ELEMENT(#16913,-3.);
#8982=DERIVED_UNIT_ELEMENT(#9042,1.);
#8983=DERIVED_UNIT_ELEMENT(#16913,-3.);
#8984=DERIVED_UNIT_ELEMENT(#9042,1.);
#8985=DERIVED_UNIT_ELEMENT(#16913,-3.);
#8986=DERIVED_UNIT_ELEMENT(#9042,1.);
#8987=DERIVED_UNIT_ELEMENT(#16913,-3.);
#8988=DERIVED_UNIT_ELEMENT(#9042,1.);
#8989=DERIVED_UNIT_ELEMENT(#16913,-3.);
#8990=DERIVED_UNIT_ELEMENT(#9042,1.);
#8991=DERIVED_UNIT_ELEMENT(#16913,-3.);
#8992=DERIVED_UNIT_ELEMENT(#9042,1.);
#8993=DERIVED_UNIT_ELEMENT(#16913,-3.);
#8994=DERIVED_UNIT_ELEMENT(#9042,1.);
#8995=DERIVED_UNIT_ELEMENT(#16913,-3.);
#8996=DERIVED_UNIT_ELEMENT(#9042,1.);
#8997=DERIVED_UNIT_ELEMENT(#16913,-3.);
#8998=DERIVED_UNIT_ELEMENT(#9042,1.);
#8999=DERIVED_UNIT_ELEMENT(#16913,-3.);
#9000=DERIVED_UNIT_ELEMENT(#9042,1.);
#9001=DERIVED_UNIT_ELEMENT(#16913,-3.);
#9002=DERIVED_UNIT_ELEMENT(#9042,1.);
#9003=DERIVED_UNIT_ELEMENT(#16913,-3.);
#9004=DERIVED_UNIT_ELEMENT(#9042,1.);
#9005=DERIVED_UNIT_ELEMENT(#16913,-3.);
#9006=DERIVED_UNIT_ELEMENT(#9042,1.);
#9007=DERIVED_UNIT_ELEMENT(#16913,-3.);
#9008=DERIVED_UNIT_ELEMENT(#9042,1.);
#9009=DERIVED_UNIT_ELEMENT(#16913,-3.);
#9010=DERIVED_UNIT_ELEMENT(#9042,1.);
#9011=DERIVED_UNIT_ELEMENT(#16913,-3.);
#9012=DERIVED_UNIT_ELEMENT(#9042,1.);
#9013=DERIVED_UNIT_ELEMENT(#16913,-3.);
#9014=DERIVED_UNIT_ELEMENT(#9042,1.);
#9015=DERIVED_UNIT_ELEMENT(#16913,-3.);
#9016=DERIVED_UNIT_ELEMENT(#9042,1.);
#9017=DERIVED_UNIT_ELEMENT(#16913,-3.);
#9018=DERIVED_UNIT_ELEMENT(#9042,1.);
#9019=DERIVED_UNIT_ELEMENT(#16913,-3.);
#9020=DERIVED_UNIT_ELEMENT(#9042,1.);
#9021=DERIVED_UNIT_ELEMENT(#16913,-3.);
#9022=DERIVED_UNIT_ELEMENT(#9042,1.);
#9023=DERIVED_UNIT_ELEMENT(#16913,-3.);
#9024=DERIVED_UNIT_ELEMENT(#9042,1.);
#9025=DERIVED_UNIT_ELEMENT(#16913,-3.);
#9026=DERIVED_UNIT_ELEMENT(#9042,1.);
#9027=DERIVED_UNIT_ELEMENT(#16913,-3.);
#9028=DERIVED_UNIT_ELEMENT(#9042,1.);
#9029=DERIVED_UNIT_ELEMENT(#16913,-3.);
#9030=DERIVED_UNIT_ELEMENT(#9042,1.);
#9031=DERIVED_UNIT_ELEMENT(#16913,-3.);
#9032=DERIVED_UNIT_ELEMENT(#9042,1.);
#9033=DERIVED_UNIT_ELEMENT(#16913,-3.);
#9034=DERIVED_UNIT_ELEMENT(#9042,1.);
#9035=DERIVED_UNIT_ELEMENT(#16913,-3.);
#9036=DERIVED_UNIT_ELEMENT(#9042,1.);
#9037=DERIVED_UNIT_ELEMENT(#16913,-3.);
#9038=DERIVED_UNIT_ELEMENT(#9042,1.);
#9039=DERIVED_UNIT_ELEMENT(#16913,-3.);
#9040=DERIVED_UNIT_ELEMENT(#9042,1.);
#9041=DERIVED_UNIT_ELEMENT(#16913,-3.);
#9042=(
MASS_UNIT()
NAMED_UNIT(*)
SI_UNIT(.KILO.,.GRAM.)
);
#9043=DERIVED_UNIT((#8942,#8943));
#9044=DERIVED_UNIT((#8944,#8945));
#9045=DERIVED_UNIT((#8946,#8947));
#9046=DERIVED_UNIT((#8948,#8949));
#9047=DERIVED_UNIT((#8950,#8951));
#9048=DERIVED_UNIT((#8952,#8953));
#9049=DERIVED_UNIT((#8954,#8955));
#9050=DERIVED_UNIT((#8956,#8957));
#9051=DERIVED_UNIT((#8958,#8959));
#9052=DERIVED_UNIT((#8960,#8961));
#9053=DERIVED_UNIT((#8962,#8963));
#9054=DERIVED_UNIT((#8964,#8965));
#9055=DERIVED_UNIT((#8966,#8967));
#9056=DERIVED_UNIT((#8968,#8969));
#9057=DERIVED_UNIT((#8970,#8971));
#9058=DERIVED_UNIT((#8972,#8973));
#9059=DERIVED_UNIT((#8974,#8975));
#9060=DERIVED_UNIT((#8976,#8977));
#9061=DERIVED_UNIT((#8978,#8979));
#9062=DERIVED_UNIT((#8980,#8981));
#9063=DERIVED_UNIT((#8982,#8983));
#9064=DERIVED_UNIT((#8984,#8985));
#9065=DERIVED_UNIT((#8986,#8987));
#9066=DERIVED_UNIT((#8988,#8989));
#9067=DERIVED_UNIT((#8990,#8991));
#9068=DERIVED_UNIT((#8992,#8993));
#9069=DERIVED_UNIT((#8994,#8995));
#9070=DERIVED_UNIT((#8996,#8997));
#9071=DERIVED_UNIT((#8998,#8999));
#9072=DERIVED_UNIT((#9000,#9001));
#9073=DERIVED_UNIT((#9002,#9003));
#9074=DERIVED_UNIT((#9004,#9005));
#9075=DERIVED_UNIT((#9006,#9007));
#9076=DERIVED_UNIT((#9008,#9009));
#9077=DERIVED_UNIT((#9010,#9011));
#9078=DERIVED_UNIT((#9012,#9013));
#9079=DERIVED_UNIT((#9014,#9015));
#9080=DERIVED_UNIT((#9016,#9017));
#9081=DERIVED_UNIT((#9018,#9019));
#9082=DERIVED_UNIT((#9020,#9021));
#9083=DERIVED_UNIT((#9022,#9023));
#9084=DERIVED_UNIT((#9024,#9025));
#9085=DERIVED_UNIT((#9026,#9027));
#9086=DERIVED_UNIT((#9028,#9029));
#9087=DERIVED_UNIT((#9030,#9031));
#9088=DERIVED_UNIT((#9032,#9033));
#9089=DERIVED_UNIT((#9034,#9035));
#9090=DERIVED_UNIT((#9036,#9037));
#9091=DERIVED_UNIT((#9038,#9039));
#9092=DERIVED_UNIT((#9040,#9041));
#9093=MEASURE_REPRESENTATION_ITEM('density measure',
POSITIVE_RATIO_MEASURE(7850.),#9043);
#9094=MEASURE_REPRESENTATION_ITEM('density measure',
POSITIVE_RATIO_MEASURE(7850.),#9044);
#9095=MEASURE_REPRESENTATION_ITEM('density measure',
POSITIVE_RATIO_MEASURE(7850.),#9045);
#9096=MEASURE_REPRESENTATION_ITEM('density measure',
POSITIVE_RATIO_MEASURE(7850.),#9046);
#9097=MEASURE_REPRESENTATION_ITEM('density measure',
POSITIVE_RATIO_MEASURE(7850.),#9047);
#9098=MEASURE_REPRESENTATION_ITEM('density measure',
POSITIVE_RATIO_MEASURE(7850.),#9048);
#9099=MEASURE_REPRESENTATION_ITEM('density measure',
POSITIVE_RATIO_MEASURE(7850.),#9049);
#9100=MEASURE_REPRESENTATION_ITEM('density measure',
POSITIVE_RATIO_MEASURE(7850.),#9050);
#9101=MEASURE_REPRESENTATION_ITEM('density measure',
POSITIVE_RATIO_MEASURE(7850.),#9051);
#9102=MEASURE_REPRESENTATION_ITEM('density measure',
POSITIVE_RATIO_MEASURE(7850.),#9052);
#9103=MEASURE_REPRESENTATION_ITEM('density measure',
POSITIVE_RATIO_MEASURE(7850.),#9053);
#9104=MEASURE_REPRESENTATION_ITEM('density measure',
POSITIVE_RATIO_MEASURE(7850.),#9054);
#9105=MEASURE_REPRESENTATION_ITEM('density measure',
POSITIVE_RATIO_MEASURE(7850.),#9055);
#9106=MEASURE_REPRESENTATION_ITEM('density measure',
POSITIVE_RATIO_MEASURE(7850.),#9056);
#9107=MEASURE_REPRESENTATION_ITEM('density measure',
POSITIVE_RATIO_MEASURE(7850.),#9057);
#9108=MEASURE_REPRESENTATION_ITEM('density measure',
POSITIVE_RATIO_MEASURE(7850.),#9058);
#9109=MEASURE_REPRESENTATION_ITEM('density measure',
POSITIVE_RATIO_MEASURE(7850.),#9059);
#9110=MEASURE_REPRESENTATION_ITEM('density measure',
POSITIVE_RATIO_MEASURE(7850.),#9060);
#9111=MEASURE_REPRESENTATION_ITEM('density measure',
POSITIVE_RATIO_MEASURE(7850.),#9061);
#9112=MEASURE_REPRESENTATION_ITEM('density measure',
POSITIVE_RATIO_MEASURE(7850.),#9062);
#9113=MEASURE_REPRESENTATION_ITEM('density measure',
POSITIVE_RATIO_MEASURE(7850.),#9063);
#9114=MEASURE_REPRESENTATION_ITEM('density measure',
POSITIVE_RATIO_MEASURE(7850.),#9064);
#9115=MEASURE_REPRESENTATION_ITEM('density measure',
POSITIVE_RATIO_MEASURE(7850.),#9065);
#9116=MEASURE_REPRESENTATION_ITEM('density measure',
POSITIVE_RATIO_MEASURE(7850.),#9066);
#9117=MEASURE_REPRESENTATION_ITEM('density measure',
POSITIVE_RATIO_MEASURE(7850.),#9067);
#9118=MEASURE_REPRESENTATION_ITEM('density measure',
POSITIVE_RATIO_MEASURE(7850.),#9068);
#9119=MEASURE_REPRESENTATION_ITEM('density measure',
POSITIVE_RATIO_MEASURE(7850.),#9069);
#9120=MEASURE_REPRESENTATION_ITEM('density measure',
POSITIVE_RATIO_MEASURE(7850.),#9070);
#9121=MEASURE_REPRESENTATION_ITEM('density measure',
POSITIVE_RATIO_MEASURE(7850.),#9071);
#9122=MEASURE_REPRESENTATION_ITEM('density measure',
POSITIVE_RATIO_MEASURE(7850.),#9072);
#9123=MEASURE_REPRESENTATION_ITEM('density measure',
POSITIVE_RATIO_MEASURE(7850.),#9073);
#9124=MEASURE_REPRESENTATION_ITEM('density measure',
POSITIVE_RATIO_MEASURE(7850.),#9074);
#9125=MEASURE_REPRESENTATION_ITEM('density measure',
POSITIVE_RATIO_MEASURE(7850.),#9075);
#9126=MEASURE_REPRESENTATION_ITEM('density measure',
POSITIVE_RATIO_MEASURE(7850.),#9076);
#9127=MEASURE_REPRESENTATION_ITEM('density measure',
POSITIVE_RATIO_MEASURE(7850.),#9077);
#9128=MEASURE_REPRESENTATION_ITEM('density measure',
POSITIVE_RATIO_MEASURE(7850.),#9078);
#9129=MEASURE_REPRESENTATION_ITEM('density measure',
POSITIVE_RATIO_MEASURE(7850.),#9079);
#9130=MEASURE_REPRESENTATION_ITEM('density measure',
POSITIVE_RATIO_MEASURE(7850.),#9080);
#9131=MEASURE_REPRESENTATION_ITEM('density measure',
POSITIVE_RATIO_MEASURE(7850.),#9081);
#9132=MEASURE_REPRESENTATION_ITEM('density measure',
POSITIVE_RATIO_MEASURE(7850.),#9082);
#9133=MEASURE_REPRESENTATION_ITEM('density measure',
POSITIVE_RATIO_MEASURE(7850.),#9083);
#9134=MEASURE_REPRESENTATION_ITEM('density measure',
POSITIVE_RATIO_MEASURE(7850.),#9084);
#9135=MEASURE_REPRESENTATION_ITEM('density measure',
POSITIVE_RATIO_MEASURE(7850.),#9085);
#9136=MEASURE_REPRESENTATION_ITEM('density measure',
POSITIVE_RATIO_MEASURE(7850.),#9086);
#9137=MEASURE_REPRESENTATION_ITEM('density measure',
POSITIVE_RATIO_MEASURE(7850.),#9087);
#9138=MEASURE_REPRESENTATION_ITEM('density measure',
POSITIVE_RATIO_MEASURE(7850.),#9088);
#9139=MEASURE_REPRESENTATION_ITEM('density measure',
POSITIVE_RATIO_MEASURE(7850.),#9089);
#9140=MEASURE_REPRESENTATION_ITEM('density measure',
POSITIVE_RATIO_MEASURE(7850.),#9090);
#9141=MEASURE_REPRESENTATION_ITEM('density measure',
POSITIVE_RATIO_MEASURE(7850.),#9091);
#9142=MEASURE_REPRESENTATION_ITEM('density measure',
POSITIVE_RATIO_MEASURE(7850.),#9092);
#9143=PROPERTY_DEFINITION_REPRESENTATION(#9393,#9243);
#9144=PROPERTY_DEFINITION_REPRESENTATION(#9394,#9244);
#9145=PROPERTY_DEFINITION_REPRESENTATION(#9395,#9245);
#9146=PROPERTY_DEFINITION_REPRESENTATION(#9396,#9246);
#9147=PROPERTY_DEFINITION_REPRESENTATION(#9397,#9247);
#9148=PROPERTY_DEFINITION_REPRESENTATION(#9398,#9248);
#9149=PROPERTY_DEFINITION_REPRESENTATION(#9399,#9249);
#9150=PROPERTY_DEFINITION_REPRESENTATION(#9400,#9250);
#9151=PROPERTY_DEFINITION_REPRESENTATION(#9401,#9251);
#9152=PROPERTY_DEFINITION_REPRESENTATION(#9402,#9252);
#9153=PROPERTY_DEFINITION_REPRESENTATION(#9403,#9253);
#9154=PROPERTY_DEFINITION_REPRESENTATION(#9404,#9254);
#9155=PROPERTY_DEFINITION_REPRESENTATION(#9405,#9255);
#9156=PROPERTY_DEFINITION_REPRESENTATION(#9406,#9256);
#9157=PROPERTY_DEFINITION_REPRESENTATION(#9407,#9257);
#9158=PROPERTY_DEFINITION_REPRESENTATION(#9408,#9258);
#9159=PROPERTY_DEFINITION_REPRESENTATION(#9409,#9259);
#9160=PROPERTY_DEFINITION_REPRESENTATION(#9410,#9260);
#9161=PROPERTY_DEFINITION_REPRESENTATION(#9411,#9261);
#9162=PROPERTY_DEFINITION_REPRESENTATION(#9412,#9262);
#9163=PROPERTY_DEFINITION_REPRESENTATION(#9413,#9263);
#9164=PROPERTY_DEFINITION_REPRESENTATION(#9414,#9264);
#9165=PROPERTY_DEFINITION_REPRESENTATION(#9415,#9265);
#9166=PROPERTY_DEFINITION_REPRESENTATION(#9416,#9266);
#9167=PROPERTY_DEFINITION_REPRESENTATION(#9417,#9267);
#9168=PROPERTY_DEFINITION_REPRESENTATION(#9418,#9268);
#9169=PROPERTY_DEFINITION_REPRESENTATION(#9419,#9269);
#9170=PROPERTY_DEFINITION_REPRESENTATION(#9420,#9270);
#9171=PROPERTY_DEFINITION_REPRESENTATION(#9421,#9271);
#9172=PROPERTY_DEFINITION_REPRESENTATION(#9422,#9272);
#9173=PROPERTY_DEFINITION_REPRESENTATION(#9423,#9273);
#9174=PROPERTY_DEFINITION_REPRESENTATION(#9424,#9274);
#9175=PROPERTY_DEFINITION_REPRESENTATION(#9425,#9275);
#9176=PROPERTY_DEFINITION_REPRESENTATION(#9426,#9276);
#9177=PROPERTY_DEFINITION_REPRESENTATION(#9427,#9277);
#9178=PROPERTY_DEFINITION_REPRESENTATION(#9428,#9278);
#9179=PROPERTY_DEFINITION_REPRESENTATION(#9429,#9279);
#9180=PROPERTY_DEFINITION_REPRESENTATION(#9430,#9280);
#9181=PROPERTY_DEFINITION_REPRESENTATION(#9431,#9281);
#9182=PROPERTY_DEFINITION_REPRESENTATION(#9432,#9282);
#9183=PROPERTY_DEFINITION_REPRESENTATION(#9433,#9283);
#9184=PROPERTY_DEFINITION_REPRESENTATION(#9434,#9284);
#9185=PROPERTY_DEFINITION_REPRESENTATION(#9435,#9285);
#9186=PROPERTY_DEFINITION_REPRESENTATION(#9436,#9286);
#9187=PROPERTY_DEFINITION_REPRESENTATION(#9437,#9287);
#9188=PROPERTY_DEFINITION_REPRESENTATION(#9438,#9288);
#9189=PROPERTY_DEFINITION_REPRESENTATION(#9439,#9289);
#9190=PROPERTY_DEFINITION_REPRESENTATION(#9440,#9290);
#9191=PROPERTY_DEFINITION_REPRESENTATION(#9441,#9291);
#9192=PROPERTY_DEFINITION_REPRESENTATION(#9442,#9292);
#9193=PROPERTY_DEFINITION_REPRESENTATION(#9443,#9293);
#9194=PROPERTY_DEFINITION_REPRESENTATION(#9444,#9294);
#9195=PROPERTY_DEFINITION_REPRESENTATION(#9445,#9295);
#9196=PROPERTY_DEFINITION_REPRESENTATION(#9446,#9296);
#9197=PROPERTY_DEFINITION_REPRESENTATION(#9447,#9297);
#9198=PROPERTY_DEFINITION_REPRESENTATION(#9448,#9298);
#9199=PROPERTY_DEFINITION_REPRESENTATION(#9449,#9299);
#9200=PROPERTY_DEFINITION_REPRESENTATION(#9450,#9300);
#9201=PROPERTY_DEFINITION_REPRESENTATION(#9451,#9301);
#9202=PROPERTY_DEFINITION_REPRESENTATION(#9452,#9302);
#9203=PROPERTY_DEFINITION_REPRESENTATION(#9453,#9303);
#9204=PROPERTY_DEFINITION_REPRESENTATION(#9454,#9304);
#9205=PROPERTY_DEFINITION_REPRESENTATION(#9455,#9305);
#9206=PROPERTY_DEFINITION_REPRESENTATION(#9456,#9306);
#9207=PROPERTY_DEFINITION_REPRESENTATION(#9457,#9307);
#9208=PROPERTY_DEFINITION_REPRESENTATION(#9458,#9308);
#9209=PROPERTY_DEFINITION_REPRESENTATION(#9459,#9309);
#9210=PROPERTY_DEFINITION_REPRESENTATION(#9460,#9310);
#9211=PROPERTY_DEFINITION_REPRESENTATION(#9461,#9311);
#9212=PROPERTY_DEFINITION_REPRESENTATION(#9462,#9312);
#9213=PROPERTY_DEFINITION_REPRESENTATION(#9463,#9313);
#9214=PROPERTY_DEFINITION_REPRESENTATION(#9464,#9314);
#9215=PROPERTY_DEFINITION_REPRESENTATION(#9465,#9315);
#9216=PROPERTY_DEFINITION_REPRESENTATION(#9466,#9316);
#9217=PROPERTY_DEFINITION_REPRESENTATION(#9467,#9317);
#9218=PROPERTY_DEFINITION_REPRESENTATION(#9468,#9318);
#9219=PROPERTY_DEFINITION_REPRESENTATION(#9469,#9319);
#9220=PROPERTY_DEFINITION_REPRESENTATION(#9470,#9320);
#9221=PROPERTY_DEFINITION_REPRESENTATION(#9471,#9321);
#9222=PROPERTY_DEFINITION_REPRESENTATION(#9472,#9322);
#9223=PROPERTY_DEFINITION_REPRESENTATION(#9473,#9323);
#9224=PROPERTY_DEFINITION_REPRESENTATION(#9474,#9324);
#9225=PROPERTY_DEFINITION_REPRESENTATION(#9475,#9325);
#9226=PROPERTY_DEFINITION_REPRESENTATION(#9476,#9326);
#9227=PROPERTY_DEFINITION_REPRESENTATION(#9477,#9327);
#9228=PROPERTY_DEFINITION_REPRESENTATION(#9478,#9328);
#9229=PROPERTY_DEFINITION_REPRESENTATION(#9479,#9329);
#9230=PROPERTY_DEFINITION_REPRESENTATION(#9480,#9330);
#9231=PROPERTY_DEFINITION_REPRESENTATION(#9481,#9331);
#9232=PROPERTY_DEFINITION_REPRESENTATION(#9482,#9332);
#9233=PROPERTY_DEFINITION_REPRESENTATION(#9483,#9333);
#9234=PROPERTY_DEFINITION_REPRESENTATION(#9484,#9334);
#9235=PROPERTY_DEFINITION_REPRESENTATION(#9485,#9335);
#9236=PROPERTY_DEFINITION_REPRESENTATION(#9486,#9336);
#9237=PROPERTY_DEFINITION_REPRESENTATION(#9487,#9337);
#9238=PROPERTY_DEFINITION_REPRESENTATION(#9488,#9338);
#9239=PROPERTY_DEFINITION_REPRESENTATION(#9489,#9339);
#9240=PROPERTY_DEFINITION_REPRESENTATION(#9490,#9340);
#9241=PROPERTY_DEFINITION_REPRESENTATION(#9491,#9341);
#9242=PROPERTY_DEFINITION_REPRESENTATION(#9492,#9342);
#9243=REPRESENTATION('material name',(#9343),#16855);
#9244=REPRESENTATION('density',(#9093),#16855);
#9245=REPRESENTATION('material name',(#9344),#16856);
#9246=REPRESENTATION('density',(#9094),#16856);
#9247=REPRESENTATION('material name',(#9345),#16857);
#9248=REPRESENTATION('density',(#9095),#16857);
#9249=REPRESENTATION('material name',(#9346),#16858);
#9250=REPRESENTATION('density',(#9096),#16858);
#9251=REPRESENTATION('material name',(#9347),#16859);
#9252=REPRESENTATION('density',(#9097),#16859);
#9253=REPRESENTATION('material name',(#9348),#16860);
#9254=REPRESENTATION('density',(#9098),#16860);
#9255=REPRESENTATION('material name',(#9349),#16861);
#9256=REPRESENTATION('density',(#9099),#16861);
#9257=REPRESENTATION('material name',(#9350),#16862);
#9258=REPRESENTATION('density',(#9100),#16862);
#9259=REPRESENTATION('material name',(#9351),#16863);
#9260=REPRESENTATION('density',(#9101),#16863);
#9261=REPRESENTATION('material name',(#9352),#16864);
#9262=REPRESENTATION('density',(#9102),#16864);
#9263=REPRESENTATION('material name',(#9353),#16866);
#9264=REPRESENTATION('density',(#9103),#16866);
#9265=REPRESENTATION('material name',(#9354),#16867);
#9266=REPRESENTATION('density',(#9104),#16867);
#9267=REPRESENTATION('material name',(#9355),#16868);
#9268=REPRESENTATION('density',(#9105),#16868);
#9269=REPRESENTATION('material name',(#9356),#16869);
#9270=REPRESENTATION('density',(#9106),#16869);
#9271=REPRESENTATION('material name',(#9357),#16870);
#9272=REPRESENTATION('density',(#9107),#16870);
#9273=REPRESENTATION('material name',(#9358),#16871);
#9274=REPRESENTATION('density',(#9108),#16871);
#9275=REPRESENTATION('material name',(#9359),#16873);
#9276=REPRESENTATION('density',(#9109),#16873);
#9277=REPRESENTATION('material name',(#9360),#16874);
#9278=REPRESENTATION('density',(#9110),#16874);
#9279=REPRESENTATION('material name',(#9361),#16875);
#9280=REPRESENTATION('density',(#9111),#16875);
#9281=REPRESENTATION('material name',(#9362),#16876);
#9282=REPRESENTATION('density',(#9112),#16876);
#9283=REPRESENTATION('material name',(#9363),#16877);
#9284=REPRESENTATION('density',(#9113),#16877);
#9285=REPRESENTATION('material name',(#9364),#16878);
#9286=REPRESENTATION('density',(#9114),#16878);
#9287=REPRESENTATION('material name',(#9365),#16879);
#9288=REPRESENTATION('density',(#9115),#16879);
#9289=REPRESENTATION('material name',(#9366),#16880);
#9290=REPRESENTATION('density',(#9116),#16880);
#9291=REPRESENTATION('material name',(#9367),#16881);
#9292=REPRESENTATION('density',(#9117),#16881);
#9293=REPRESENTATION('material name',(#9368),#16882);
#9294=REPRESENTATION('density',(#9118),#16882);
#9295=REPRESENTATION('material name',(#9369),#16883);
#9296=REPRESENTATION('density',(#9119),#16883);
#9297=REPRESENTATION('material name',(#9370),#16885);
#9298=REPRESENTATION('density',(#9120),#16885);
#9299=REPRESENTATION('material name',(#9371),#16886);
#9300=REPRESENTATION('density',(#9121),#16886);
#9301=REPRESENTATION('material name',(#9372),#16887);
#9302=REPRESENTATION('density',(#9122),#16887);
#9303=REPRESENTATION('material name',(#9373),#16888);
#9304=REPRESENTATION('density',(#9123),#16888);
#9305=REPRESENTATION('material name',(#9374),#16889);
#9306=REPRESENTATION('density',(#9124),#16889);
#9307=REPRESENTATION('material name',(#9375),#16891);
#9308=REPRESENTATION('density',(#9125),#16891);
#9309=REPRESENTATION('material name',(#9376),#16892);
#9310=REPRESENTATION('density',(#9126),#16892);
#9311=REPRESENTATION('material name',(#9377),#16893);
#9312=REPRESENTATION('density',(#9127),#16893);
#9313=REPRESENTATION('material name',(#9378),#16894);
#9314=REPRESENTATION('density',(#9128),#16894);
#9315=REPRESENTATION('material name',(#9379),#16895);
#9316=REPRESENTATION('density',(#9129),#16895);
#9317=REPRESENTATION('material name',(#9380),#16897);
#9318=REPRESENTATION('density',(#9130),#16897);
#9319=REPRESENTATION('material name',(#9381),#16898);
#9320=REPRESENTATION('density',(#9131),#16898);
#9321=REPRESENTATION('material name',(#9382),#16899);
#9322=REPRESENTATION('density',(#9132),#16899);
#9323=REPRESENTATION('material name',(#9383),#16900);
#9324=REPRESENTATION('density',(#9133),#16900);
#9325=REPRESENTATION('material name',(#9384),#16901);
#9326=REPRESENTATION('density',(#9134),#16901);
#9327=REPRESENTATION('material name',(#9385),#16902);
#9328=REPRESENTATION('density',(#9135),#16902);
#9329=REPRESENTATION('material name',(#9386),#16904);
#9330=REPRESENTATION('density',(#9136),#16904);
#9331=REPRESENTATION('material name',(#9387),#16905);
#9332=REPRESENTATION('density',(#9137),#16905);
#9333=REPRESENTATION('material name',(#9388),#16906);
#9334=REPRESENTATION('density',(#9138),#16906);
#9335=REPRESENTATION('material name',(#9389),#16907);
#9336=REPRESENTATION('density',(#9139),#16907);
#9337=REPRESENTATION('material name',(#9390),#16908);
#9338=REPRESENTATION('density',(#9140),#16908);
#9339=REPRESENTATION('material name',(#9391),#16909);
#9340=REPRESENTATION('density',(#9141),#16909);
#9341=REPRESENTATION('material name',(#9392),#16910);
#9342=REPRESENTATION('density',(#9142),#16910);
#9343=DESCRIPTIVE_REPRESENTATION_ITEM('Steel','Steel');
#9344=DESCRIPTIVE_REPRESENTATION_ITEM('Steel','Steel');
#9345=DESCRIPTIVE_REPRESENTATION_ITEM('Steel','Steel');
#9346=DESCRIPTIVE_REPRESENTATION_ITEM('Steel','Steel');
#9347=DESCRIPTIVE_REPRESENTATION_ITEM('Steel','Steel');
#9348=DESCRIPTIVE_REPRESENTATION_ITEM('Steel','Steel');
#9349=DESCRIPTIVE_REPRESENTATION_ITEM('Steel','Steel');
#9350=DESCRIPTIVE_REPRESENTATION_ITEM('Steel','Steel');
#9351=DESCRIPTIVE_REPRESENTATION_ITEM('Steel','Steel');
#9352=DESCRIPTIVE_REPRESENTATION_ITEM('Steel','Steel');
#9353=DESCRIPTIVE_REPRESENTATION_ITEM('Steel','Steel');
#9354=DESCRIPTIVE_REPRESENTATION_ITEM('Steel','Steel');
#9355=DESCRIPTIVE_REPRESENTATION_ITEM('Steel','Steel');
#9356=DESCRIPTIVE_REPRESENTATION_ITEM('Steel','Steel');
#9357=DESCRIPTIVE_REPRESENTATION_ITEM('Steel','Steel');
#9358=DESCRIPTIVE_REPRESENTATION_ITEM('Steel','Steel');
#9359=DESCRIPTIVE_REPRESENTATION_ITEM('Steel','Steel');
#9360=DESCRIPTIVE_REPRESENTATION_ITEM('Steel','Steel');
#9361=DESCRIPTIVE_REPRESENTATION_ITEM('Steel','Steel');
#9362=DESCRIPTIVE_REPRESENTATION_ITEM('Steel','Steel');
#9363=DESCRIPTIVE_REPRESENTATION_ITEM('Steel','Steel');
#9364=DESCRIPTIVE_REPRESENTATION_ITEM('Steel','Steel');
#9365=DESCRIPTIVE_REPRESENTATION_ITEM('Steel','Steel');
#9366=DESCRIPTIVE_REPRESENTATION_ITEM('Steel','Steel');
#9367=DESCRIPTIVE_REPRESENTATION_ITEM('Steel','Steel');
#9368=DESCRIPTIVE_REPRESENTATION_ITEM('Steel','Steel');
#9369=DESCRIPTIVE_REPRESENTATION_ITEM('Steel','Steel');
#9370=DESCRIPTIVE_REPRESENTATION_ITEM('Steel','Steel');
#9371=DESCRIPTIVE_REPRESENTATION_ITEM('Steel','Steel');
#9372=DESCRIPTIVE_REPRESENTATION_ITEM('Steel','Steel');
#9373=DESCRIPTIVE_REPRESENTATION_ITEM('Steel','Steel');
#9374=DESCRIPTIVE_REPRESENTATION_ITEM('Steel','Steel');
#9375=DESCRIPTIVE_REPRESENTATION_ITEM('Steel','Steel');
#9376=DESCRIPTIVE_REPRESENTATION_ITEM('Steel','Steel');
#9377=DESCRIPTIVE_REPRESENTATION_ITEM('Steel','Steel');
#9378=DESCRIPTIVE_REPRESENTATION_ITEM('Steel','Steel');
#9379=DESCRIPTIVE_REPRESENTATION_ITEM('Steel','Steel');
#9380=DESCRIPTIVE_REPRESENTATION_ITEM('Steel','Steel');
#9381=DESCRIPTIVE_REPRESENTATION_ITEM('Steel','Steel');
#9382=DESCRIPTIVE_REPRESENTATION_ITEM('Steel','Steel');
#9383=DESCRIPTIVE_REPRESENTATION_ITEM('Steel','Steel');
#9384=DESCRIPTIVE_REPRESENTATION_ITEM('Steel','Steel');
#9385=DESCRIPTIVE_REPRESENTATION_ITEM('Steel','Steel');
#9386=DESCRIPTIVE_REPRESENTATION_ITEM('Steel','Steel');
#9387=DESCRIPTIVE_REPRESENTATION_ITEM('Steel','Steel');
#9388=DESCRIPTIVE_REPRESENTATION_ITEM('Steel','Steel');
#9389=DESCRIPTIVE_REPRESENTATION_ITEM('Steel','Steel');
#9390=DESCRIPTIVE_REPRESENTATION_ITEM('Steel','Steel');
#9391=DESCRIPTIVE_REPRESENTATION_ITEM('Steel','Steel');
#9392=DESCRIPTIVE_REPRESENTATION_ITEM('Steel','Steel');
#9393=PROPERTY_DEFINITION('material property','material name',#17185);
#9394=PROPERTY_DEFINITION('material property','density of part',#17185);
#9395=PROPERTY_DEFINITION('material property','material name',#17186);
#9396=PROPERTY_DEFINITION('material property','density of part',#17186);
#9397=PROPERTY_DEFINITION('material property','material name',#17187);
#9398=PROPERTY_DEFINITION('material property','density of part',#17187);
#9399=PROPERTY_DEFINITION('material property','material name',#17188);
#9400=PROPERTY_DEFINITION('material property','density of part',#17188);
#9401=PROPERTY_DEFINITION('material property','material name',#17189);
#9402=PROPERTY_DEFINITION('material property','density of part',#17189);
#9403=PROPERTY_DEFINITION('material property','material name',#17190);
#9404=PROPERTY_DEFINITION('material property','density of part',#17190);
#9405=PROPERTY_DEFINITION('material property','material name',#17191);
#9406=PROPERTY_DEFINITION('material property','density of part',#17191);
#9407=PROPERTY_DEFINITION('material property','material name',#17192);
#9408=PROPERTY_DEFINITION('material property','density of part',#17192);
#9409=PROPERTY_DEFINITION('material property','material name',#17193);
#9410=PROPERTY_DEFINITION('material property','density of part',#17193);
#9411=PROPERTY_DEFINITION('material property','material name',#17194);
#9412=PROPERTY_DEFINITION('material property','density of part',#17194);
#9413=PROPERTY_DEFINITION('material property','material name',#17196);
#9414=PROPERTY_DEFINITION('material property','density of part',#17196);
#9415=PROPERTY_DEFINITION('material property','material name',#17197);
#9416=PROPERTY_DEFINITION('material property','density of part',#17197);
#9417=PROPERTY_DEFINITION('material property','material name',#17198);
#9418=PROPERTY_DEFINITION('material property','density of part',#17198);
#9419=PROPERTY_DEFINITION('material property','material name',#17199);
#9420=PROPERTY_DEFINITION('material property','density of part',#17199);
#9421=PROPERTY_DEFINITION('material property','material name',#17200);
#9422=PROPERTY_DEFINITION('material property','density of part',#17200);
#9423=PROPERTY_DEFINITION('material property','material name',#17201);
#9424=PROPERTY_DEFINITION('material property','density of part',#17201);
#9425=PROPERTY_DEFINITION('material property','material name',#17203);
#9426=PROPERTY_DEFINITION('material property','density of part',#17203);
#9427=PROPERTY_DEFINITION('material property','material name',#17204);
#9428=PROPERTY_DEFINITION('material property','density of part',#17204);
#9429=PROPERTY_DEFINITION('material property','material name',#17205);
#9430=PROPERTY_DEFINITION('material property','density of part',#17205);
#9431=PROPERTY_DEFINITION('material property','material name',#17206);
#9432=PROPERTY_DEFINITION('material property','density of part',#17206);
#9433=PROPERTY_DEFINITION('material property','material name',#17207);
#9434=PROPERTY_DEFINITION('material property','density of part',#17207);
#9435=PROPERTY_DEFINITION('material property','material name',#17208);
#9436=PROPERTY_DEFINITION('material property','density of part',#17208);
#9437=PROPERTY_DEFINITION('material property','material name',#17209);
#9438=PROPERTY_DEFINITION('material property','density of part',#17209);
#9439=PROPERTY_DEFINITION('material property','material name',#17210);
#9440=PROPERTY_DEFINITION('material property','density of part',#17210);
#9441=PROPERTY_DEFINITION('material property','material name',#17211);
#9442=PROPERTY_DEFINITION('material property','density of part',#17211);
#9443=PROPERTY_DEFINITION('material property','material name',#17212);
#9444=PROPERTY_DEFINITION('material property','density of part',#17212);
#9445=PROPERTY_DEFINITION('material property','material name',#17213);
#9446=PROPERTY_DEFINITION('material property','density of part',#17213);
#9447=PROPERTY_DEFINITION('material property','material name',#17215);
#9448=PROPERTY_DEFINITION('material property','density of part',#17215);
#9449=PROPERTY_DEFINITION('material property','material name',#17216);
#9450=PROPERTY_DEFINITION('material property','density of part',#17216);
#9451=PROPERTY_DEFINITION('material property','material name',#17217);
#9452=PROPERTY_DEFINITION('material property','density of part',#17217);
#9453=PROPERTY_DEFINITION('material property','material name',#17218);
#9454=PROPERTY_DEFINITION('material property','density of part',#17218);
#9455=PROPERTY_DEFINITION('material property','material name',#17219);
#9456=PROPERTY_DEFINITION('material property','density of part',#17219);
#9457=PROPERTY_DEFINITION('material property','material name',#17221);
#9458=PROPERTY_DEFINITION('material property','density of part',#17221);
#9459=PROPERTY_DEFINITION('material property','material name',#17222);
#9460=PROPERTY_DEFINITION('material property','density of part',#17222);
#9461=PROPERTY_DEFINITION('material property','material name',#17223);
#9462=PROPERTY_DEFINITION('material property','density of part',#17223);
#9463=PROPERTY_DEFINITION('material property','material name',#17224);
#9464=PROPERTY_DEFINITION('material property','density of part',#17224);
#9465=PROPERTY_DEFINITION('material property','material name',#17225);
#9466=PROPERTY_DEFINITION('material property','density of part',#17225);
#9467=PROPERTY_DEFINITION('material property','material name',#17227);
#9468=PROPERTY_DEFINITION('material property','density of part',#17227);
#9469=PROPERTY_DEFINITION('material property','material name',#17228);
#9470=PROPERTY_DEFINITION('material property','density of part',#17228);
#9471=PROPERTY_DEFINITION('material property','material name',#17229);
#9472=PROPERTY_DEFINITION('material property','density of part',#17229);
#9473=PROPERTY_DEFINITION('material property','material name',#17230);
#9474=PROPERTY_DEFINITION('material property','density of part',#17230);
#9475=PROPERTY_DEFINITION('material property','material name',#17231);
#9476=PROPERTY_DEFINITION('material property','density of part',#17231);
#9477=PROPERTY_DEFINITION('material property','material name',#17232);
#9478=PROPERTY_DEFINITION('material property','density of part',#17232);
#9479=PROPERTY_DEFINITION('material property','material name',#17234);
#9480=PROPERTY_DEFINITION('material property','density of part',#17234);
#9481=PROPERTY_DEFINITION('material property','material name',#17235);
#9482=PROPERTY_DEFINITION('material property','density of part',#17235);
#9483=PROPERTY_DEFINITION('material property','material name',#17236);
#9484=PROPERTY_DEFINITION('material property','density of part',#17236);
#9485=PROPERTY_DEFINITION('material property','material name',#17237);
#9486=PROPERTY_DEFINITION('material property','density of part',#17237);
#9487=PROPERTY_DEFINITION('material property','material name',#17238);
#9488=PROPERTY_DEFINITION('material property','density of part',#17238);
#9489=PROPERTY_DEFINITION('material property','material name',#17239);
#9490=PROPERTY_DEFINITION('material property','density of part',#17239);
#9491=PROPERTY_DEFINITION('material property','material name',#17240);
#9492=PROPERTY_DEFINITION('material property','density of part',#17240);
#9493=AXIS2_PLACEMENT_3D('',#13358,#10566,#10567);
#9494=AXIS2_PLACEMENT_3D('',#13359,#10568,#10569);
#9495=AXIS2_PLACEMENT_3D('',#13360,#10570,#10571);
#9496=AXIS2_PLACEMENT_3D('',#13361,#10572,#10573);
#9497=AXIS2_PLACEMENT_3D('',#13363,#10574,#10575);
#9498=AXIS2_PLACEMENT_3D('',#13366,#10577,#10578);
#9499=AXIS2_PLACEMENT_3D('',#13367,#10579,#10580);
#9500=AXIS2_PLACEMENT_3D('',#13369,#10581,#10582);
#9501=AXIS2_PLACEMENT_3D('',#13372,#10584,#10585);
#9502=AXIS2_PLACEMENT_3D('',#13373,#10586,#10587);
#9503=AXIS2_PLACEMENT_3D('',#13375,#10588,#10589);
#9504=AXIS2_PLACEMENT_3D('',#13378,#10591,#10592);
#9505=AXIS2_PLACEMENT_3D('',#13379,#10593,#10594);
#9506=AXIS2_PLACEMENT_3D('',#13381,#10595,#10596);
#9507=AXIS2_PLACEMENT_3D('',#13384,#10598,#10599);
#9508=AXIS2_PLACEMENT_3D('',#13385,#10600,#10601);
#9509=AXIS2_PLACEMENT_3D('',#13387,#10602,#10603);
#9510=AXIS2_PLACEMENT_3D('',#13390,#10605,#10606);
#9511=AXIS2_PLACEMENT_3D('',#13391,#10607,#10608);
#9512=AXIS2_PLACEMENT_3D('',#13393,#10609,#10610);
#9513=AXIS2_PLACEMENT_3D('',#13396,#10612,#10613);
#9514=AXIS2_PLACEMENT_3D('',#13397,#10614,#10615);
#9515=AXIS2_PLACEMENT_3D('',#13399,#10616,#10617);
#9516=AXIS2_PLACEMENT_3D('',#13402,#10619,#10620);
#9517=AXIS2_PLACEMENT_3D('',#13403,#10621,#10622);
#9518=AXIS2_PLACEMENT_3D('',#13405,#10623,#10624);
#9519=AXIS2_PLACEMENT_3D('',#13408,#10626,#10627);
#9520=AXIS2_PLACEMENT_3D('',#13409,#10628,#10629);
#9521=AXIS2_PLACEMENT_3D('',#13411,#10630,#10631);
#9522=AXIS2_PLACEMENT_3D('',#13414,#10633,#10634);
#9523=AXIS2_PLACEMENT_3D('',#13415,#10635,#10636);
#9524=AXIS2_PLACEMENT_3D('',#13417,#10637,#10638);
#9525=AXIS2_PLACEMENT_3D('',#13420,#10640,#10641);
#9526=AXIS2_PLACEMENT_3D('',#13421,#10642,#10643);
#9527=AXIS2_PLACEMENT_3D('',#13423,#10644,#10645);
#9528=AXIS2_PLACEMENT_3D('',#13426,#10647,#10648);
#9529=AXIS2_PLACEMENT_3D('',#13427,#10649,#10650);
#9530=AXIS2_PLACEMENT_3D('',#13429,#10651,#10652);
#9531=AXIS2_PLACEMENT_3D('',#13432,#10654,#10655);
#9532=AXIS2_PLACEMENT_3D('',#13433,#10656,#10657);
#9533=AXIS2_PLACEMENT_3D('',#13442,#10662,#10663);
#9534=AXIS2_PLACEMENT_3D('',#13448,#10667,#10668);
#9535=AXIS2_PLACEMENT_3D('',#13454,#10672,#10673);
#9536=AXIS2_PLACEMENT_3D('',#13457,#10676,#10677);
#9537=AXIS2_PLACEMENT_3D('',#13458,#10678,#10679);
#9538=AXIS2_PLACEMENT_3D('',#13459,#10680,#10681);
#9539=AXIS2_PLACEMENT_3D('',#13460,#10682,#10683);
#9540=AXIS2_PLACEMENT_3D('',#13462,#10684,#10685);
#9541=AXIS2_PLACEMENT_3D('',#13465,#10687,#10688);
#9542=AXIS2_PLACEMENT_3D('',#13466,#10689,#10690);
#9543=AXIS2_PLACEMENT_3D('',#13467,#10691,#10692);
#9544=AXIS2_PLACEMENT_3D('',#13469,#10693,#10694);
#9545=AXIS2_PLACEMENT_3D('',#13472,#10696,#10697);
#9546=AXIS2_PLACEMENT_3D('',#13473,#10698,#10699);
#9547=AXIS2_PLACEMENT_3D('',#13474,#10700,#10701);
#9548=AXIS2_PLACEMENT_3D('',#13476,#10702,#10703);
#9549=AXIS2_PLACEMENT_3D('',#13479,#10705,#10706);
#9550=AXIS2_PLACEMENT_3D('',#13480,#10707,#10708);
#9551=AXIS2_PLACEMENT_3D('',#13482,#10709,#10710);
#9552=AXIS2_PLACEMENT_3D('',#13483,#10711,#10712);
#9553=AXIS2_PLACEMENT_3D('',#13485,#10713,#10714);
#9554=AXIS2_PLACEMENT_3D('',#13488,#10716,#10717);
#9555=AXIS2_PLACEMENT_3D('',#13489,#10718,#10719);
#9556=AXIS2_PLACEMENT_3D('',#13491,#10720,#10721);
#9557=AXIS2_PLACEMENT_3D('',#13492,#10722,#10723);
#9558=AXIS2_PLACEMENT_3D('',#13494,#10724,#10725);
#9559=AXIS2_PLACEMENT_3D('',#13497,#10727,#10728);
#9560=AXIS2_PLACEMENT_3D('',#13498,#10729,#10730);
#9561=AXIS2_PLACEMENT_3D('',#13500,#10731,#10732);
#9562=AXIS2_PLACEMENT_3D('',#13501,#10733,#10734);
#9563=AXIS2_PLACEMENT_3D('',#13503,#10735,#10736);
#9564=AXIS2_PLACEMENT_3D('',#13506,#10738,#10739);
#9565=AXIS2_PLACEMENT_3D('',#13507,#10740,#10741);
#9566=AXIS2_PLACEMENT_3D('',#13509,#10742,#10743);
#9567=AXIS2_PLACEMENT_3D('',#13510,#10744,#10745);
#9568=AXIS2_PLACEMENT_3D('',#13512,#10746,#10747);
#9569=AXIS2_PLACEMENT_3D('',#13514,#10749,#10750);
#9570=AXIS2_PLACEMENT_3D('',#13516,#10751,#10752);
#9571=AXIS2_PLACEMENT_3D('',#13518,#10754,#10755);
#9572=AXIS2_PLACEMENT_3D('',#13520,#10756,#10757);
#9573=AXIS2_PLACEMENT_3D('',#13522,#10759,#10760);
#9574=AXIS2_PLACEMENT_3D('',#13524,#10761,#10762);
#9575=AXIS2_PLACEMENT_3D('',#13526,#10764,#10765);
#9576=AXIS2_PLACEMENT_3D('',#13535,#10770,#10771);
#9577=AXIS2_PLACEMENT_3D('',#13541,#10775,#10776);
#9578=AXIS2_PLACEMENT_3D('',#13547,#10780,#10781);
#9579=AXIS2_PLACEMENT_3D('',#13550,#10784,#10785);
#9580=AXIS2_PLACEMENT_3D('',#13551,#10786,#10787);
#9581=AXIS2_PLACEMENT_3D('',#13552,#10788,#10789);
#9582=AXIS2_PLACEMENT_3D('',#13553,#10790,#10791);
#9583=AXIS2_PLACEMENT_3D('',#13555,#10792,#10793);
#9584=AXIS2_PLACEMENT_3D('',#13558,#10795,#10796);
#9585=AXIS2_PLACEMENT_3D('',#13559,#10797,#10798);
#9586=AXIS2_PLACEMENT_3D('',#13561,#10799,#10800);
#9587=AXIS2_PLACEMENT_3D('',#13564,#10802,#10803);
#9588=AXIS2_PLACEMENT_3D('',#13565,#10804,#10805);
#9589=AXIS2_PLACEMENT_3D('',#13566,#10806,#10807);
#9590=AXIS2_PLACEMENT_3D('',#13567,#10808,#10809);
#9591=AXIS2_PLACEMENT_3D('',#13568,#10810,#10811);
#9592=AXIS2_PLACEMENT_3D('',#13570,#10812,#10813);
#9593=AXIS2_PLACEMENT_3D('',#13573,#10815,#10816);
#9594=AXIS2_PLACEMENT_3D('',#13574,#10817,#10818);
#9595=AXIS2_PLACEMENT_3D('',#13576,#10819,#10820);
#9596=AXIS2_PLACEMENT_3D('',#13579,#10822,#10823);
#9597=AXIS2_PLACEMENT_3D('',#13580,#10824,#10825);
#9598=AXIS2_PLACEMENT_3D('',#13581,#10826,#10827);
#9599=AXIS2_PLACEMENT_3D('',#13582,#10828,#10829);
#9600=AXIS2_PLACEMENT_3D('',#13583,#10830,#10831);
#9601=AXIS2_PLACEMENT_3D('',#13585,#10832,#10833);
#9602=AXIS2_PLACEMENT_3D('',#13588,#10835,#10836);
#9603=AXIS2_PLACEMENT_3D('',#13589,#10837,#10838);
#9604=AXIS2_PLACEMENT_3D('',#13590,#10839,#10840);
#9605=AXIS2_PLACEMENT_3D('',#13592,#10841,#10842);
#9606=AXIS2_PLACEMENT_3D('',#13595,#10844,#10845);
#9607=AXIS2_PLACEMENT_3D('',#13596,#10846,#10847);
#9608=AXIS2_PLACEMENT_3D('',#13597,#10848,#10849);
#9609=AXIS2_PLACEMENT_3D('',#13599,#10850,#10851);
#9610=AXIS2_PLACEMENT_3D('',#13602,#10853,#10854);
#9611=AXIS2_PLACEMENT_3D('',#13603,#10855,#10856);
#9612=AXIS2_PLACEMENT_3D('',#13605,#10857,#10858);
#9613=AXIS2_PLACEMENT_3D('',#13606,#10859,#10860);
#9614=AXIS2_PLACEMENT_3D('',#13608,#10861,#10862);
#9615=AXIS2_PLACEMENT_3D('',#13611,#10864,#10865);
#9616=AXIS2_PLACEMENT_3D('',#13612,#10866,#10867);
#9617=AXIS2_PLACEMENT_3D('',#13614,#10868,#10869);
#9618=AXIS2_PLACEMENT_3D('',#13615,#10870,#10871);
#9619=AXIS2_PLACEMENT_3D('',#13617,#10872,#10873);
#9620=AXIS2_PLACEMENT_3D('',#13620,#10875,#10876);
#9621=AXIS2_PLACEMENT_3D('',#13621,#10877,#10878);
#9622=AXIS2_PLACEMENT_3D('',#13623,#10879,#10880);
#9623=AXIS2_PLACEMENT_3D('',#13624,#10881,#10882);
#9624=AXIS2_PLACEMENT_3D('',#13626,#10883,#10884);
#9625=AXIS2_PLACEMENT_3D('',#13629,#10886,#10887);
#9626=AXIS2_PLACEMENT_3D('',#13630,#10888,#10889);
#9627=AXIS2_PLACEMENT_3D('',#13632,#10890,#10891);
#9628=AXIS2_PLACEMENT_3D('',#13633,#10892,#10893);
#9629=AXIS2_PLACEMENT_3D('',#13635,#10894,#10895);
#9630=AXIS2_PLACEMENT_3D('',#13637,#10897,#10898);
#9631=AXIS2_PLACEMENT_3D('',#13639,#10899,#10900);
#9632=AXIS2_PLACEMENT_3D('',#13641,#10902,#10903);
#9633=AXIS2_PLACEMENT_3D('',#13643,#10904,#10905);
#9634=AXIS2_PLACEMENT_3D('',#13645,#10907,#10908);
#9635=AXIS2_PLACEMENT_3D('',#13647,#10909,#10910);
#9636=AXIS2_PLACEMENT_3D('',#13649,#10912,#10913);
#9637=AXIS2_PLACEMENT_3D('',#13658,#10918,#10919);
#9638=AXIS2_PLACEMENT_3D('',#13664,#10923,#10924);
#9639=AXIS2_PLACEMENT_3D('',#13670,#10928,#10929);
#9640=AXIS2_PLACEMENT_3D('',#13673,#10932,#10933);
#9641=AXIS2_PLACEMENT_3D('',#13674,#10934,#10935);
#9642=AXIS2_PLACEMENT_3D('',#13675,#10936,#10937);
#9643=AXIS2_PLACEMENT_3D('',#13676,#10938,#10939);
#9644=AXIS2_PLACEMENT_3D('',#13678,#10940,#10941);
#9645=AXIS2_PLACEMENT_3D('',#13681,#10943,#10944);
#9646=AXIS2_PLACEMENT_3D('',#13682,#10945,#10946);
#9647=AXIS2_PLACEMENT_3D('',#13684,#10947,#10948);
#9648=AXIS2_PLACEMENT_3D('',#13687,#10950,#10951);
#9649=AXIS2_PLACEMENT_3D('',#13688,#10952,#10953);
#9650=AXIS2_PLACEMENT_3D('',#13689,#10954,#10955);
#9651=AXIS2_PLACEMENT_3D('',#13690,#10956,#10957);
#9652=AXIS2_PLACEMENT_3D('',#13691,#10958,#10959);
#9653=AXIS2_PLACEMENT_3D('',#13693,#10960,#10961);
#9654=AXIS2_PLACEMENT_3D('',#13696,#10963,#10964);
#9655=AXIS2_PLACEMENT_3D('',#13697,#10965,#10966);
#9656=AXIS2_PLACEMENT_3D('',#13699,#10967,#10968);
#9657=AXIS2_PLACEMENT_3D('',#13702,#10970,#10971);
#9658=AXIS2_PLACEMENT_3D('',#13703,#10972,#10973);
#9659=AXIS2_PLACEMENT_3D('',#13704,#10974,#10975);
#9660=AXIS2_PLACEMENT_3D('',#13705,#10976,#10977);
#9661=AXIS2_PLACEMENT_3D('',#13706,#10978,#10979);
#9662=AXIS2_PLACEMENT_3D('',#13708,#10980,#10981);
#9663=AXIS2_PLACEMENT_3D('',#13711,#10983,#10984);
#9664=AXIS2_PLACEMENT_3D('',#13712,#10985,#10986);
#9665=AXIS2_PLACEMENT_3D('',#13713,#10987,#10988);
#9666=AXIS2_PLACEMENT_3D('',#13715,#10989,#10990);
#9667=AXIS2_PLACEMENT_3D('',#13718,#10992,#10993);
#9668=AXIS2_PLACEMENT_3D('',#13719,#10994,#10995);
#9669=AXIS2_PLACEMENT_3D('',#13720,#10996,#10997);
#9670=AXIS2_PLACEMENT_3D('',#13722,#10998,#10999);
#9671=AXIS2_PLACEMENT_3D('',#13725,#11001,#11002);
#9672=AXIS2_PLACEMENT_3D('',#13726,#11003,#11004);
#9673=AXIS2_PLACEMENT_3D('',#13727,#11005,#11006);
#9674=AXIS2_PLACEMENT_3D('',#13729,#11007,#11008);
#9675=AXIS2_PLACEMENT_3D('',#13732,#11010,#11011);
#9676=AXIS2_PLACEMENT_3D('',#13733,#11012,#11013);
#9677=AXIS2_PLACEMENT_3D('',#13734,#11014,#11015);
#9678=AXIS2_PLACEMENT_3D('',#13736,#11016,#11017);
#9679=AXIS2_PLACEMENT_3D('',#13739,#11019,#11020);
#9680=AXIS2_PLACEMENT_3D('',#13740,#11021,#11022);
#9681=AXIS2_PLACEMENT_3D('',#13742,#11023,#11024);
#9682=AXIS2_PLACEMENT_3D('',#13743,#11025,#11026);
#9683=AXIS2_PLACEMENT_3D('',#13745,#11027,#11028);
#9684=AXIS2_PLACEMENT_3D('',#13748,#11030,#11031);
#9685=AXIS2_PLACEMENT_3D('',#13749,#11032,#11033);
#9686=AXIS2_PLACEMENT_3D('',#13751,#11034,#11035);
#9687=AXIS2_PLACEMENT_3D('',#13752,#11036,#11037);
#9688=AXIS2_PLACEMENT_3D('',#13754,#11038,#11039);
#9689=AXIS2_PLACEMENT_3D('',#13757,#11041,#11042);
#9690=AXIS2_PLACEMENT_3D('',#13758,#11043,#11044);
#9691=AXIS2_PLACEMENT_3D('',#13760,#11045,#11046);
#9692=AXIS2_PLACEMENT_3D('',#13761,#11047,#11048);
#9693=AXIS2_PLACEMENT_3D('',#13763,#11049,#11050);
#9694=AXIS2_PLACEMENT_3D('',#13766,#11052,#11053);
#9695=AXIS2_PLACEMENT_3D('',#13767,#11054,#11055);
#9696=AXIS2_PLACEMENT_3D('',#13769,#11056,#11057);
#9697=AXIS2_PLACEMENT_3D('',#13770,#11058,#11059);
#9698=AXIS2_PLACEMENT_3D('',#13772,#11060,#11061);
#9699=AXIS2_PLACEMENT_3D('',#13774,#11063,#11064);
#9700=AXIS2_PLACEMENT_3D('',#13776,#11065,#11066);
#9701=AXIS2_PLACEMENT_3D('',#13778,#11068,#11069);
#9702=AXIS2_PLACEMENT_3D('',#13780,#11070,#11071);
#9703=AXIS2_PLACEMENT_3D('',#13782,#11073,#11074);
#9704=AXIS2_PLACEMENT_3D('',#13784,#11075,#11076);
#9705=AXIS2_PLACEMENT_3D('',#13786,#11078,#11079);
#9706=AXIS2_PLACEMENT_3D('',#13795,#11084,#11085);
#9707=AXIS2_PLACEMENT_3D('',#13801,#11089,#11090);
#9708=AXIS2_PLACEMENT_3D('',#13807,#11094,#11095);
#9709=AXIS2_PLACEMENT_3D('',#13810,#11098,#11099);
#9710=AXIS2_PLACEMENT_3D('',#13811,#11100,#11101);
#9711=AXIS2_PLACEMENT_3D('',#13812,#11102,#11103);
#9712=AXIS2_PLACEMENT_3D('',#13813,#11104,#11105);
#9713=AXIS2_PLACEMENT_3D('',#13822,#11110,#11111);
#9714=AXIS2_PLACEMENT_3D('',#13828,#11115,#11116);
#9715=AXIS2_PLACEMENT_3D('',#13834,#11120,#11121);
#9716=AXIS2_PLACEMENT_3D('',#13837,#11124,#11125);
#9717=AXIS2_PLACEMENT_3D('',#13838,#11126,#11127);
#9718=AXIS2_PLACEMENT_3D('',#13839,#11128,#11129);
#9719=AXIS2_PLACEMENT_3D('',#13840,#11130,#11131);
#9720=AXIS2_PLACEMENT_3D('',#13849,#11136,#11137);
#9721=AXIS2_PLACEMENT_3D('',#13855,#11141,#11142);
#9722=AXIS2_PLACEMENT_3D('',#13861,#11146,#11147);
#9723=AXIS2_PLACEMENT_3D('',#13864,#11150,#11151);
#9724=AXIS2_PLACEMENT_3D('',#13865,#11152,#11153);
#9725=AXIS2_PLACEMENT_3D('',#13866,#11154,#11155);
#9726=AXIS2_PLACEMENT_3D('',#13867,#11156,#11157);
#9727=AXIS2_PLACEMENT_3D('',#13868,#11158,#11159);
#9728=AXIS2_PLACEMENT_3D('',#13870,#11160,#11161);
#9729=AXIS2_PLACEMENT_3D('',#13873,#11163,#11164);
#9730=AXIS2_PLACEMENT_3D('',#13874,#11165,#11166);
#9731=AXIS2_PLACEMENT_3D('',#13876,#11167,#11168);
#9732=AXIS2_PLACEMENT_3D('',#13879,#11170,#11171);
#9733=AXIS2_PLACEMENT_3D('',#13880,#11172,#11173);
#9734=AXIS2_PLACEMENT_3D('',#13883,#11174,#11175);
#9735=AXIS2_PLACEMENT_3D('',#13884,#11176,#11177);
#9736=AXIS2_PLACEMENT_3D('',#13890,#11180,#11181);
#9737=AXIS2_PLACEMENT_3D('',#13891,#11182,#11183);
#9738=AXIS2_PLACEMENT_3D('',#13896,#11185,#11186);
#9739=AXIS2_PLACEMENT_3D('',#13898,#11188,#11189);
#9740=AXIS2_PLACEMENT_3D('',#13903,#11191,#11192);
#9741=AXIS2_PLACEMENT_3D('',#13905,#11194,#11195);
#9742=AXIS2_PLACEMENT_3D('',#13908,#11198,#11199);
#9743=AXIS2_PLACEMENT_3D('',#13914,#11202,#11203);
#9744=AXIS2_PLACEMENT_3D('',#13915,#11204,#11205);
#9745=AXIS2_PLACEMENT_3D('',#13918,#11208,#11209);
#9746=AXIS2_PLACEMENT_3D('',#13928,#11214,#11215);
#9747=AXIS2_PLACEMENT_3D('',#13930,#11216,#11217);
#9748=AXIS2_PLACEMENT_3D('',#13941,#11224,#11225);
#9749=AXIS2_PLACEMENT_3D('',#13942,#11226,#11227);
#9750=AXIS2_PLACEMENT_3D('',#13943,#11228,#11229);
#9751=AXIS2_PLACEMENT_3D('',#13944,#11230,#11231);
#9752=AXIS2_PLACEMENT_3D('',#13945,#11232,#11233);
#9753=AXIS2_PLACEMENT_3D('',#13946,#11234,#11235);
#9754=AXIS2_PLACEMENT_3D('',#13955,#11240,#11241);
#9755=AXIS2_PLACEMENT_3D('',#13961,#11245,#11246);
#9756=AXIS2_PLACEMENT_3D('',#13967,#11250,#11251);
#9757=AXIS2_PLACEMENT_3D('',#13970,#11254,#11255);
#9758=AXIS2_PLACEMENT_3D('',#13971,#11256,#11257);
#9759=AXIS2_PLACEMENT_3D('',#13973,#11258,#11259);
#9760=AXIS2_PLACEMENT_3D('',#13975,#11261,#11262);
#9761=AXIS2_PLACEMENT_3D('',#13977,#11263,#11264);
#9762=AXIS2_PLACEMENT_3D('',#13979,#11266,#11267);
#9763=AXIS2_PLACEMENT_3D('',#13985,#11271,#11272);
#9764=AXIS2_PLACEMENT_3D('',#13989,#11275,#11276);
#9765=AXIS2_PLACEMENT_3D('',#13993,#11279,#11280);
#9766=AXIS2_PLACEMENT_3D('',#13995,#11282,#11283);
#9767=AXIS2_PLACEMENT_3D('',#13996,#11284,#11285);
#9768=AXIS2_PLACEMENT_3D('',#13997,#11286,#11287);
#9769=AXIS2_PLACEMENT_3D('',#13999,#11288,#11289);
#9770=AXIS2_PLACEMENT_3D('',#14002,#11291,#11292);
#9771=AXIS2_PLACEMENT_3D('',#14003,#11293,#11294);
#9772=AXIS2_PLACEMENT_3D('',#14005,#11295,#11296);
#9773=AXIS2_PLACEMENT_3D('',#14006,#11297,#11298);
#9774=AXIS2_PLACEMENT_3D('',#14009,#11299,#11300);
#9775=AXIS2_PLACEMENT_3D('',#14011,#11301,#11302);
#9776=AXIS2_PLACEMENT_3D('',#14012,#11303,#11304);
#9777=AXIS2_PLACEMENT_3D('',#14013,#11305,#11306);
#9778=AXIS2_PLACEMENT_3D('',#14091,#11308,#11309);
#9779=AXIS2_PLACEMENT_3D('',#14169,#11311,#11312);
#9780=AXIS2_PLACEMENT_3D('',#14171,#11313,#11314);
#9781=AXIS2_PLACEMENT_3D('',#14174,#11316,#11317);
#9782=AXIS2_PLACEMENT_3D('',#14339,#11318,#11319);
#9783=AXIS2_PLACEMENT_3D('',#14376,#11321,#11322);
#9784=AXIS2_PLACEMENT_3D('',#14413,#11324,#11325);
#9785=AXIS2_PLACEMENT_3D('',#14450,#11327,#11328);
#9786=AXIS2_PLACEMENT_3D('',#14487,#11330,#11331);
#9787=AXIS2_PLACEMENT_3D('',#14489,#11332,#11333);
#9788=AXIS2_PLACEMENT_3D('',#14490,#11334,#11335);
#9789=AXIS2_PLACEMENT_3D('',#14492,#11336,#11337);
#9790=AXIS2_PLACEMENT_3D('',#14493,#11338,#11339);
#9791=AXIS2_PLACEMENT_3D('',#14495,#11340,#11341);
#9792=AXIS2_PLACEMENT_3D('',#14497,#11343,#11344);
#9793=AXIS2_PLACEMENT_3D('',#14499,#11345,#11346);
#9794=AXIS2_PLACEMENT_3D('',#14500,#11347,#11348);
#9795=AXIS2_PLACEMENT_3D('',#14502,#11350,#11351);
#9796=AXIS2_PLACEMENT_3D('',#14503,#11352,#11353);
#9797=AXIS2_PLACEMENT_3D('',#14504,#11354,#11355);
#9798=AXIS2_PLACEMENT_3D('',#14505,#11356,#11357);
#9799=AXIS2_PLACEMENT_3D('',#14507,#11358,#11359);
#9800=AXIS2_PLACEMENT_3D('',#14510,#11361,#11362);
#9801=AXIS2_PLACEMENT_3D('',#14511,#11363,#11364);
#9802=AXIS2_PLACEMENT_3D('',#14513,#11365,#11366);
#9803=AXIS2_PLACEMENT_3D('',#14516,#11368,#11369);
#9804=AXIS2_PLACEMENT_3D('',#14517,#11370,#11371);
#9805=AXIS2_PLACEMENT_3D('',#14518,#11372,#11373);
#9806=AXIS2_PLACEMENT_3D('',#14519,#11374,#11375);
#9807=AXIS2_PLACEMENT_3D('',#14520,#11376,#11377);
#9808=AXIS2_PLACEMENT_3D('',#14529,#11382,#11383);
#9809=AXIS2_PLACEMENT_3D('',#14535,#11387,#11388);
#9810=AXIS2_PLACEMENT_3D('',#14541,#11392,#11393);
#9811=AXIS2_PLACEMENT_3D('',#14547,#11397,#11398);
#9812=AXIS2_PLACEMENT_3D('',#14553,#11402,#11403);
#9813=AXIS2_PLACEMENT_3D('',#14556,#11406,#11407);
#9814=AXIS2_PLACEMENT_3D('',#14557,#11408,#11409);
#9815=AXIS2_PLACEMENT_3D('',#14558,#11410,#11411);
#9816=AXIS2_PLACEMENT_3D('',#14560,#11412,#11413);
#9817=AXIS2_PLACEMENT_3D('',#14561,#11414,#11415);
#9818=AXIS2_PLACEMENT_3D('',#14563,#11416,#11417);
#9819=AXIS2_PLACEMENT_3D('',#14564,#11418,#11419);
#9820=AXIS2_PLACEMENT_3D('',#14566,#11420,#11421);
#9821=AXIS2_PLACEMENT_3D('',#14568,#11423,#11424);
#9822=AXIS2_PLACEMENT_3D('',#14570,#11425,#11426);
#9823=AXIS2_PLACEMENT_3D('',#14572,#11428,#11429);
#9824=AXIS2_PLACEMENT_3D('',#14574,#11430,#11431);
#9825=AXIS2_PLACEMENT_3D('',#14576,#11433,#11434);
#9826=AXIS2_PLACEMENT_3D('',#14578,#11435,#11436);
#9827=AXIS2_PLACEMENT_3D('',#14579,#11437,#11438);
#9828=AXIS2_PLACEMENT_3D('',#14581,#11439,#11440);
#9829=AXIS2_PLACEMENT_3D('',#14583,#11442,#11443);
#9830=AXIS2_PLACEMENT_3D('',#14585,#11445,#11446);
#9831=AXIS2_PLACEMENT_3D('',#14586,#11447,#11448);
#9832=AXIS2_PLACEMENT_3D('',#14588,#11449,#11450);
#9833=AXIS2_PLACEMENT_3D('',#14591,#11452,#11453);
#9834=AXIS2_PLACEMENT_3D('',#14592,#11454,#11455);
#9835=AXIS2_PLACEMENT_3D('',#14594,#11456,#11457);
#9836=AXIS2_PLACEMENT_3D('',#14595,#11458,#11459);
#9837=AXIS2_PLACEMENT_3D('',#14597,#11460,#11461);
#9838=AXIS2_PLACEMENT_3D('',#14600,#11463,#11464);
#9839=AXIS2_PLACEMENT_3D('',#14601,#11465,#11466);
#9840=AXIS2_PLACEMENT_3D('',#14603,#11467,#11468);
#9841=AXIS2_PLACEMENT_3D('',#14604,#11469,#11470);
#9842=AXIS2_PLACEMENT_3D('',#14606,#11471,#11472);
#9843=AXIS2_PLACEMENT_3D('',#14609,#11474,#11475);
#9844=AXIS2_PLACEMENT_3D('',#14610,#11476,#11477);
#9845=AXIS2_PLACEMENT_3D('',#14612,#11478,#11479);
#9846=AXIS2_PLACEMENT_3D('',#14613,#11480,#11481);
#9847=AXIS2_PLACEMENT_3D('',#14615,#11482,#11483);
#9848=AXIS2_PLACEMENT_3D('',#14618,#11485,#11486);
#9849=AXIS2_PLACEMENT_3D('',#14619,#11487,#11488);
#9850=AXIS2_PLACEMENT_3D('',#14621,#11489,#11490);
#9851=AXIS2_PLACEMENT_3D('',#14622,#11491,#11492);
#9852=AXIS2_PLACEMENT_3D('',#14624,#11493,#11494);
#9853=AXIS2_PLACEMENT_3D('',#14626,#11496,#11497);
#9854=AXIS2_PLACEMENT_3D('',#14628,#11498,#11499);
#9855=AXIS2_PLACEMENT_3D('',#14630,#11501,#11502);
#9856=AXIS2_PLACEMENT_3D('',#14632,#11503,#11504);
#9857=AXIS2_PLACEMENT_3D('',#14634,#11506,#11507);
#9858=AXIS2_PLACEMENT_3D('',#14636,#11508,#11509);
#9859=AXIS2_PLACEMENT_3D('',#14638,#11511,#11512);
#9860=AXIS2_PLACEMENT_3D('',#14647,#11517,#11518);
#9861=AXIS2_PLACEMENT_3D('',#14653,#11522,#11523);
#9862=AXIS2_PLACEMENT_3D('',#14659,#11527,#11528);
#9863=AXIS2_PLACEMENT_3D('',#14665,#11532,#11533);
#9864=AXIS2_PLACEMENT_3D('',#14671,#11537,#11538);
#9865=AXIS2_PLACEMENT_3D('',#14677,#11542,#11543);
#9866=AXIS2_PLACEMENT_3D('',#14683,#11547,#11548);
#9867=AXIS2_PLACEMENT_3D('',#14689,#11552,#11553);
#9868=AXIS2_PLACEMENT_3D('',#14695,#11557,#11558);
#9869=AXIS2_PLACEMENT_3D('',#14701,#11562,#11563);
#9870=AXIS2_PLACEMENT_3D('',#14707,#11567,#11568);
#9871=AXIS2_PLACEMENT_3D('',#14710,#11571,#11572);
#9872=AXIS2_PLACEMENT_3D('',#14711,#11573,#11574);
#9873=AXIS2_PLACEMENT_3D('',#14712,#11575,#11576);
#9874=AXIS2_PLACEMENT_3D('',#14713,#11577,#11578);
#9875=AXIS2_PLACEMENT_3D('',#14715,#11579,#11580);
#9876=AXIS2_PLACEMENT_3D('',#14716,#11581,#11582);
#9877=AXIS2_PLACEMENT_3D('',#14718,#11583,#11584);
#9878=AXIS2_PLACEMENT_3D('',#14720,#11586,#11587);
#9879=AXIS2_PLACEMENT_3D('',#14722,#11588,#11589);
#9880=AXIS2_PLACEMENT_3D('',#14724,#11591,#11592);
#9881=AXIS2_PLACEMENT_3D('',#14726,#11593,#11594);
#9882=AXIS2_PLACEMENT_3D('',#14728,#11596,#11597);
#9883=AXIS2_PLACEMENT_3D('',#14730,#11598,#11599);
#9884=AXIS2_PLACEMENT_3D('',#14731,#11600,#11601);
#9885=AXIS2_PLACEMENT_3D('',#14733,#11602,#11603);
#9886=AXIS2_PLACEMENT_3D('',#14735,#11605,#11606);
#9887=AXIS2_PLACEMENT_3D('',#14737,#11607,#11608);
#9888=AXIS2_PLACEMENT_3D('',#14739,#11610,#11611);
#9889=AXIS2_PLACEMENT_3D('',#14741,#11612,#11613);
#9890=AXIS2_PLACEMENT_3D('',#14743,#11615,#11616);
#9891=AXIS2_PLACEMENT_3D('',#14744,#11617,#11618);
#9892=AXIS2_PLACEMENT_3D('',#14753,#11623,#11624);
#9893=AXIS2_PLACEMENT_3D('',#14759,#11628,#11629);
#9894=AXIS2_PLACEMENT_3D('',#14765,#11633,#11634);
#9895=AXIS2_PLACEMENT_3D('',#14771,#11638,#11639);
#9896=AXIS2_PLACEMENT_3D('',#14777,#11643,#11644);
#9897=AXIS2_PLACEMENT_3D('',#14780,#11647,#11648);
#9898=AXIS2_PLACEMENT_3D('',#14781,#11649,#11650);
#9899=AXIS2_PLACEMENT_3D('',#14782,#11651,#11652);
#9900=AXIS2_PLACEMENT_3D('',#14783,#11653,#11654);
#9901=AXIS2_PLACEMENT_3D('',#14784,#11655,#11656);
#9902=AXIS2_PLACEMENT_3D('',#14793,#11661,#11662);
#9903=AXIS2_PLACEMENT_3D('',#14795,#11663,#11664);
#9904=AXIS2_PLACEMENT_3D('',#14799,#11667,#11668);
#9905=AXIS2_PLACEMENT_3D('',#14805,#11672,#11673);
#9906=AXIS2_PLACEMENT_3D('',#14807,#11675,#11676);
#9907=AXIS2_PLACEMENT_3D('',#14809,#11677,#11678);
#9908=AXIS2_PLACEMENT_3D('',#14812,#11680,#11681);
#9909=AXIS2_PLACEMENT_3D('',#14813,#11682,#11683);
#9910=AXIS2_PLACEMENT_3D('',#14814,#11684,#11685);
#9911=AXIS2_PLACEMENT_3D('',#14815,#11686,#11687);
#9912=AXIS2_PLACEMENT_3D('',#14816,#11688,#11689);
#9913=AXIS2_PLACEMENT_3D('',#14817,#11690,#11691);
#9914=AXIS2_PLACEMENT_3D('',#14821,#11693,#11694);
#9915=AXIS2_PLACEMENT_3D('',#14822,#11695,#11696);
#9916=AXIS2_PLACEMENT_3D('',#14839,#11697,#11698);
#9917=AXIS2_PLACEMENT_3D('',#14880,#11700,#11701);
#9918=AXIS2_PLACEMENT_3D('',#14895,#11702,#11703);
#9919=AXIS2_PLACEMENT_3D('',#14897,#11705,#11706);
#9920=AXIS2_PLACEMENT_3D('',#14899,#11707,#11708);
#9921=AXIS2_PLACEMENT_3D('',#14902,#11710,#11711);
#9922=AXIS2_PLACEMENT_3D('',#14903,#11712,#11713);
#9923=AXIS2_PLACEMENT_3D('',#14905,#11714,#11715);
#9924=AXIS2_PLACEMENT_3D('',#14908,#11717,#11718);
#9925=AXIS2_PLACEMENT_3D('',#14909,#11719,#11720);
#9926=AXIS2_PLACEMENT_3D('',#14910,#11721,#11722);
#9927=AXIS2_PLACEMENT_3D('',#14911,#11723,#11724);
#9928=AXIS2_PLACEMENT_3D('',#14912,#11725,#11726);
#9929=AXIS2_PLACEMENT_3D('',#14916,#11728,#11729);
#9930=AXIS2_PLACEMENT_3D('',#14917,#11730,#11731);
#9931=AXIS2_PLACEMENT_3D('',#14934,#11732,#11733);
#9932=AXIS2_PLACEMENT_3D('',#14975,#11735,#11736);
#9933=AXIS2_PLACEMENT_3D('',#14990,#11737,#11738);
#9934=AXIS2_PLACEMENT_3D('',#14992,#11740,#11741);
#9935=AXIS2_PLACEMENT_3D('',#14994,#11742,#11743);
#9936=AXIS2_PLACEMENT_3D('',#14997,#11745,#11746);
#9937=AXIS2_PLACEMENT_3D('',#14998,#11747,#11748);
#9938=AXIS2_PLACEMENT_3D('',#15000,#11749,#11750);
#9939=AXIS2_PLACEMENT_3D('',#15003,#11752,#11753);
#9940=AXIS2_PLACEMENT_3D('',#15004,#11754,#11755);
#9941=AXIS2_PLACEMENT_3D('',#15005,#11756,#11757);
#9942=AXIS2_PLACEMENT_3D('',#15006,#11758,#11759);
#9943=AXIS2_PLACEMENT_3D('',#15007,#11760,#11761);
#9944=AXIS2_PLACEMENT_3D('',#15009,#11762,#11763);
#9945=AXIS2_PLACEMENT_3D('',#15012,#11765,#11766);
#9946=AXIS2_PLACEMENT_3D('',#15013,#11767,#11768);
#9947=AXIS2_PLACEMENT_3D('',#15015,#11769,#11770);
#9948=AXIS2_PLACEMENT_3D('',#15018,#11772,#11773);
#9949=AXIS2_PLACEMENT_3D('',#15019,#11774,#11775);
#9950=AXIS2_PLACEMENT_3D('',#15020,#11776,#11777);
#9951=AXIS2_PLACEMENT_3D('',#15021,#11778,#11779);
#9952=AXIS2_PLACEMENT_3D('',#15022,#11780,#11781);
#9953=AXIS2_PLACEMENT_3D('',#15025,#11782,#11783);
#9954=AXIS2_PLACEMENT_3D('',#15026,#11784,#11785);
#9955=AXIS2_PLACEMENT_3D('',#15027,#11786,#11787);
#9956=AXIS2_PLACEMENT_3D('',#15031,#11789,#11790);
#9957=AXIS2_PLACEMENT_3D('',#15034,#11792,#11793);
#9958=AXIS2_PLACEMENT_3D('',#15036,#11794,#11795);
#9959=AXIS2_PLACEMENT_3D('',#15038,#11797,#11798);
#9960=AXIS2_PLACEMENT_3D('',#15040,#11799,#11800);
#9961=AXIS2_PLACEMENT_3D('',#15044,#11802,#11803);
#9962=AXIS2_PLACEMENT_3D('',#15075,#11806,#11807);
#9963=AXIS2_PLACEMENT_3D('',#15078,#11809,#11810);
#9964=AXIS2_PLACEMENT_3D('',#15079,#11811,#11812);
#9965=AXIS2_PLACEMENT_3D('',#15085,#11816,#11817);
#9966=AXIS2_PLACEMENT_3D('',#15087,#11818,#11819);
#9967=AXIS2_PLACEMENT_3D('',#15088,#11820,#11821);
#9968=AXIS2_PLACEMENT_3D('',#15094,#11825,#11826);
#9969=AXIS2_PLACEMENT_3D('',#15096,#11828,#11829);
#9970=AXIS2_PLACEMENT_3D('',#15097,#11830,#11831);
#9971=AXIS2_PLACEMENT_3D('',#15098,#11832,#11833);
#9972=AXIS2_PLACEMENT_3D('',#15099,#11834,#11835);
#9973=AXIS2_PLACEMENT_3D('',#15139,#11838,#11839);
#9974=AXIS2_PLACEMENT_3D('',#15140,#11840,#11841);
#9975=AXIS2_PLACEMENT_3D('',#15142,#11843,#11844);
#9976=AXIS2_PLACEMENT_3D('',#15144,#11845,#11846);
#9977=AXIS2_PLACEMENT_3D('',#15146,#11847,#11848);
#9978=AXIS2_PLACEMENT_3D('',#15147,#11849,#11850);
#9979=AXIS2_PLACEMENT_3D('',#15149,#11852,#11853);
#9980=AXIS2_PLACEMENT_3D('',#15152,#11855,#11856);
#9981=AXIS2_PLACEMENT_3D('',#15153,#11857,#11858);
#9982=AXIS2_PLACEMENT_3D('',#15154,#11859,#11860);
#9983=AXIS2_PLACEMENT_3D('',#15155,#11861,#11862);
#9984=AXIS2_PLACEMENT_3D('',#15156,#11863,#11864);
#9985=AXIS2_PLACEMENT_3D('',#15158,#11865,#11866);
#9986=AXIS2_PLACEMENT_3D('',#15161,#11868,#11869);
#9987=AXIS2_PLACEMENT_3D('',#15162,#11870,#11871);
#9988=AXIS2_PLACEMENT_3D('',#15163,#11872,#11873);
#9989=AXIS2_PLACEMENT_3D('',#15165,#11874,#11875);
#9990=AXIS2_PLACEMENT_3D('',#15167,#11876,#11877);
#9991=AXIS2_PLACEMENT_3D('',#15168,#11878,#11879);
#9992=AXIS2_PLACEMENT_3D('',#15170,#11880,#11881);
#9993=AXIS2_PLACEMENT_3D('',#15172,#11883,#11884);
#9994=AXIS2_PLACEMENT_3D('',#15173,#11885,#11886);
#9995=AXIS2_PLACEMENT_3D('',#15176,#11888,#11889);
#9996=AXIS2_PLACEMENT_3D('',#15177,#11890,#11891);
#9997=AXIS2_PLACEMENT_3D('',#15178,#11892,#11893);
#9998=AXIS2_PLACEMENT_3D('',#15179,#11894,#11895);
#9999=AXIS2_PLACEMENT_3D('',#15181,#11896,#11897);
#10000=AXIS2_PLACEMENT_3D('',#15184,#11899,#11900);
#10001=AXIS2_PLACEMENT_3D('',#15185,#11901,#11902);
#10002=AXIS2_PLACEMENT_3D('',#15187,#11903,#11904);
#10003=AXIS2_PLACEMENT_3D('',#15190,#11906,#11907);
#10004=AXIS2_PLACEMENT_3D('',#15191,#11908,#11909);
#10005=AXIS2_PLACEMENT_3D('',#15192,#11910,#11911);
#10006=AXIS2_PLACEMENT_3D('',#15193,#11912,#11913);
#10007=AXIS2_PLACEMENT_3D('',#15194,#11914,#11915);
#10008=AXIS2_PLACEMENT_3D('',#15196,#11916,#11917);
#10009=AXIS2_PLACEMENT_3D('',#15199,#11919,#11920);
#10010=AXIS2_PLACEMENT_3D('',#15200,#11921,#11922);
#10011=AXIS2_PLACEMENT_3D('',#15202,#11923,#11924);
#10012=AXIS2_PLACEMENT_3D('',#15205,#11926,#11927);
#10013=AXIS2_PLACEMENT_3D('',#15206,#11928,#11929);
#10014=AXIS2_PLACEMENT_3D('',#15207,#11930,#11931);
#10015=AXIS2_PLACEMENT_3D('',#15208,#11932,#11933);
#10016=AXIS2_PLACEMENT_3D('',#15209,#11934,#11935);
#10017=AXIS2_PLACEMENT_3D('',#15211,#11936,#11937);
#10018=AXIS2_PLACEMENT_3D('',#15214,#11939,#11940);
#10019=AXIS2_PLACEMENT_3D('',#15215,#11941,#11942);
#10020=AXIS2_PLACEMENT_3D('',#15217,#11943,#11944);
#10021=AXIS2_PLACEMENT_3D('',#15220,#11946,#11947);
#10022=AXIS2_PLACEMENT_3D('',#15221,#11948,#11949);
#10023=AXIS2_PLACEMENT_3D('',#15222,#11950,#11951);
#10024=AXIS2_PLACEMENT_3D('',#15223,#11952,#11953);
#10025=AXIS2_PLACEMENT_3D('',#15224,#11954,#11955);
#10026=AXIS2_PLACEMENT_3D('',#15241,#11964,#11965);
#10027=AXIS2_PLACEMENT_3D('',#15247,#11969,#11970);
#10028=AXIS2_PLACEMENT_3D('',#15251,#11973,#11974);
#10029=AXIS2_PLACEMENT_3D('',#15255,#11977,#11978);
#10030=AXIS2_PLACEMENT_3D('',#15259,#11981,#11982);
#10031=AXIS2_PLACEMENT_3D('',#15267,#11987,#11988);
#10032=AXIS2_PLACEMENT_3D('',#15269,#11990,#11991);
#10033=AXIS2_PLACEMENT_3D('',#15271,#11993,#11994);
#10034=AXIS2_PLACEMENT_3D('',#15273,#11996,#11997);
#10035=AXIS2_PLACEMENT_3D('',#15274,#11998,#11999);
#10036=AXIS2_PLACEMENT_3D('',#15275,#12000,#12001);
#10037=AXIS2_PLACEMENT_3D('',#15284,#12006,#12007);
#10038=AXIS2_PLACEMENT_3D('',#15290,#12011,#12012);
#10039=AXIS2_PLACEMENT_3D('',#15296,#12016,#12017);
#10040=AXIS2_PLACEMENT_3D('',#15302,#12021,#12022);
#10041=AXIS2_PLACEMENT_3D('',#15308,#12026,#12027);
#10042=AXIS2_PLACEMENT_3D('',#15311,#12030,#12031);
#10043=AXIS2_PLACEMENT_3D('',#15312,#12032,#12033);
#10044=AXIS2_PLACEMENT_3D('',#15314,#12034,#12035);
#10045=AXIS2_PLACEMENT_3D('',#15315,#12036,#12037);
#10046=AXIS2_PLACEMENT_3D('',#15317,#12038,#12039);
#10047=AXIS2_PLACEMENT_3D('',#15319,#12041,#12042);
#10048=AXIS2_PLACEMENT_3D('',#15321,#12043,#12044);
#10049=AXIS2_PLACEMENT_3D('',#15323,#12046,#12047);
#10050=AXIS2_PLACEMENT_3D('',#15325,#12048,#12049);
#10051=AXIS2_PLACEMENT_3D('',#15327,#12051,#12052);
#10052=AXIS2_PLACEMENT_3D('',#15328,#12053,#12054);
#10053=AXIS2_PLACEMENT_3D('',#15329,#12055,#12056);
#10054=AXIS2_PLACEMENT_3D('',#15330,#12057,#12058);
#10055=AXIS2_PLACEMENT_3D('',#15332,#12059,#12060);
#10056=AXIS2_PLACEMENT_3D('',#15335,#12062,#12063);
#10057=AXIS2_PLACEMENT_3D('',#15336,#12064,#12065);
#10058=AXIS2_PLACEMENT_3D('',#15338,#12066,#12067);
#10059=AXIS2_PLACEMENT_3D('',#15341,#12069,#12070);
#10060=AXIS2_PLACEMENT_3D('',#15342,#12071,#12072);
#10061=AXIS2_PLACEMENT_3D('',#15347,#12074,#12075);
#10062=AXIS2_PLACEMENT_3D('',#15350,#12077,#12078);
#10063=AXIS2_PLACEMENT_3D('',#15351,#12079,#12080);
#10064=AXIS2_PLACEMENT_3D('',#15355,#12082,#12083);
#10065=AXIS2_PLACEMENT_3D('',#15357,#12085,#12086);
#10066=AXIS2_PLACEMENT_3D('',#15361,#12089,#12090);
#10067=AXIS2_PLACEMENT_3D('',#15364,#12092,#12093);
#10068=AXIS2_PLACEMENT_3D('',#15365,#12094,#12095);
#10069=AXIS2_PLACEMENT_3D('',#15367,#12097,#12098);
#10070=AXIS2_PLACEMENT_3D('',#15368,#12099,#12100);
#10071=AXIS2_PLACEMENT_3D('',#15369,#12101,#12102);
#10072=AXIS2_PLACEMENT_3D('',#15371,#12103,#12104);
#10073=AXIS2_PLACEMENT_3D('',#15374,#12106,#12107);
#10074=AXIS2_PLACEMENT_3D('',#15375,#12108,#12109);
#10075=AXIS2_PLACEMENT_3D('',#15377,#12110,#12111);
#10076=AXIS2_PLACEMENT_3D('',#15380,#12113,#12114);
#10077=AXIS2_PLACEMENT_3D('',#15381,#12115,#12116);
#10078=AXIS2_PLACEMENT_3D('',#15382,#12117,#12118);
#10079=AXIS2_PLACEMENT_3D('',#15383,#12119,#12120);
#10080=AXIS2_PLACEMENT_3D('',#15384,#12121,#12122);
#10081=AXIS2_PLACEMENT_3D('',#15386,#12123,#12124);
#10082=AXIS2_PLACEMENT_3D('',#15389,#12126,#12127);
#10083=AXIS2_PLACEMENT_3D('',#15390,#12128,#12129);
#10084=AXIS2_PLACEMENT_3D('',#15392,#12130,#12131);
#10085=AXIS2_PLACEMENT_3D('',#15395,#12133,#12134);
#10086=AXIS2_PLACEMENT_3D('',#15396,#12135,#12136);
#10087=AXIS2_PLACEMENT_3D('',#15397,#12137,#12138);
#10088=AXIS2_PLACEMENT_3D('',#15398,#12139,#12140);
#10089=AXIS2_PLACEMENT_3D('',#15399,#12141,#12142);
#10090=AXIS2_PLACEMENT_3D('',#15401,#12143,#12144);
#10091=AXIS2_PLACEMENT_3D('',#15404,#12146,#12147);
#10092=AXIS2_PLACEMENT_3D('',#15405,#12148,#12149);
#10093=AXIS2_PLACEMENT_3D('',#15407,#12150,#12151);
#10094=AXIS2_PLACEMENT_3D('',#15410,#12153,#12154);
#10095=AXIS2_PLACEMENT_3D('',#15411,#12155,#12156);
#10096=AXIS2_PLACEMENT_3D('',#15412,#12157,#12158);
#10097=AXIS2_PLACEMENT_3D('',#15413,#12159,#12160);
#10098=AXIS2_PLACEMENT_3D('',#15414,#12161,#12162);
#10099=AXIS2_PLACEMENT_3D('',#15416,#12163,#12164);
#10100=AXIS2_PLACEMENT_3D('',#15419,#12166,#12167);
#10101=AXIS2_PLACEMENT_3D('',#15420,#12168,#12169);
#10102=AXIS2_PLACEMENT_3D('',#15422,#12170,#12171);
#10103=AXIS2_PLACEMENT_3D('',#15425,#12173,#12174);
#10104=AXIS2_PLACEMENT_3D('',#15426,#12175,#12176);
#10105=AXIS2_PLACEMENT_3D('',#15427,#12177,#12178);
#10106=AXIS2_PLACEMENT_3D('',#15428,#12179,#12180);
#10107=AXIS2_PLACEMENT_3D('',#15429,#12181,#12182);
#10108=AXIS2_PLACEMENT_3D('',#15430,#12183,#12184);
#10109=AXIS2_PLACEMENT_3D('',#15433,#12185,#12186);
#10110=AXIS2_PLACEMENT_3D('',#15434,#12187,#12188);
#10111=AXIS2_PLACEMENT_3D('',#15436,#12189,#12190);
#10112=AXIS2_PLACEMENT_3D('',#15438,#12191,#12192);
#10113=AXIS2_PLACEMENT_3D('',#15439,#12193,#12194);
#10114=AXIS2_PLACEMENT_3D('',#15440,#12195,#12196);
#10115=AXIS2_PLACEMENT_3D('',#15443,#12198,#12199);
#10116=AXIS2_PLACEMENT_3D('',#15444,#12200,#12201);
#10117=AXIS2_PLACEMENT_3D('',#15446,#12202,#12203);
#10118=AXIS2_PLACEMENT_3D('',#15449,#12205,#12206);
#10119=AXIS2_PLACEMENT_3D('',#15450,#12207,#12208);
#10120=AXIS2_PLACEMENT_3D('',#15453,#12210,#12211);
#10121=AXIS2_PLACEMENT_3D('',#15454,#12212,#12213);
#10122=AXIS2_PLACEMENT_3D('',#15455,#12214,#12215);
#10123=AXIS2_PLACEMENT_3D('',#15457,#12216,#12217);
#10124=AXIS2_PLACEMENT_3D('',#15459,#12219,#12220);
#10125=AXIS2_PLACEMENT_3D('',#15461,#12221,#12222);
#10126=AXIS2_PLACEMENT_3D('',#15462,#12223,#12224);
#10127=AXIS2_PLACEMENT_3D('',#15464,#12226,#12227);
#10128=AXIS2_PLACEMENT_3D('',#15465,#12228,#12229);
#10129=AXIS2_PLACEMENT_3D('',#15468,#12230,#12231);
#10130=AXIS2_PLACEMENT_3D('',#15469,#12232,#12233);
#10131=AXIS2_PLACEMENT_3D('',#15471,#12234,#12235);
#10132=AXIS2_PLACEMENT_3D('',#15473,#12236,#12237);
#10133=AXIS2_PLACEMENT_3D('',#15474,#12238,#12239);
#10134=AXIS2_PLACEMENT_3D('',#15475,#12240,#12241);
#10135=AXIS2_PLACEMENT_3D('',#15477,#12242,#12243);
#10136=AXIS2_PLACEMENT_3D('',#15479,#12245,#12246);
#10137=AXIS2_PLACEMENT_3D('',#15481,#12247,#12248);
#10138=AXIS2_PLACEMENT_3D('',#15483,#12249,#12250);
#10139=AXIS2_PLACEMENT_3D('',#15484,#12251,#12252);
#10140=AXIS2_PLACEMENT_3D('',#15486,#12253,#12254);
#10141=AXIS2_PLACEMENT_3D('',#15488,#12256,#12257);
#10142=AXIS2_PLACEMENT_3D('',#15490,#12258,#12259);
#10143=AXIS2_PLACEMENT_3D('',#15492,#12261,#12262);
#10144=AXIS2_PLACEMENT_3D('',#15494,#12263,#12264);
#10145=AXIS2_PLACEMENT_3D('',#15496,#12266,#12267);
#10146=AXIS2_PLACEMENT_3D('',#15497,#12268,#12269);
#10147=AXIS2_PLACEMENT_3D('',#15499,#12271,#12272);
#10148=AXIS2_PLACEMENT_3D('',#15500,#12273,#12274);
#10149=AXIS2_PLACEMENT_3D('',#15503,#12275,#12276);
#10150=AXIS2_PLACEMENT_3D('',#15504,#12277,#12278);
#10151=AXIS2_PLACEMENT_3D('',#15507,#12279,#12280);
#10152=AXIS2_PLACEMENT_3D('',#15508,#12281,#12282);
#10153=AXIS2_PLACEMENT_3D('',#15511,#12283,#12284);
#10154=AXIS2_PLACEMENT_3D('',#15512,#12285,#12286);
#10155=AXIS2_PLACEMENT_3D('',#15515,#12287,#12288);
#10156=AXIS2_PLACEMENT_3D('',#15516,#12289,#12290);
#10157=AXIS2_PLACEMENT_3D('',#15519,#12291,#12292);
#10158=AXIS2_PLACEMENT_3D('',#15520,#12293,#12294);
#10159=AXIS2_PLACEMENT_3D('',#15523,#12295,#12296);
#10160=AXIS2_PLACEMENT_3D('',#15524,#12297,#12298);
#10161=AXIS2_PLACEMENT_3D('',#15527,#12299,#12300);
#10162=AXIS2_PLACEMENT_3D('',#15528,#12301,#12302);
#10163=AXIS2_PLACEMENT_3D('',#15531,#12303,#12304);
#10164=AXIS2_PLACEMENT_3D('',#15532,#12305,#12306);
#10165=AXIS2_PLACEMENT_3D('',#15533,#12307,#12308);
#10166=AXIS2_PLACEMENT_3D('',#15559,#12309,#12310);
#10167=AXIS2_PLACEMENT_3D('',#15583,#12311,#12312);
#10168=AXIS2_PLACEMENT_3D('',#15584,#12313,#12314);
#10169=AXIS2_PLACEMENT_3D('',#15586,#12315,#12316);
#10170=AXIS2_PLACEMENT_3D('',#15611,#12317,#12318);
#10171=AXIS2_PLACEMENT_3D('',#15636,#12319,#12320);
#10172=AXIS2_PLACEMENT_3D('',#15652,#12322,#12323);
#10173=AXIS2_PLACEMENT_3D('',#15667,#12324,#12325);
#10174=AXIS2_PLACEMENT_3D('',#15692,#12326,#12327);
#10175=AXIS2_PLACEMENT_3D('',#15717,#12328,#12329);
#10176=AXIS2_PLACEMENT_3D('',#15742,#12330,#12331);
#10177=AXIS2_PLACEMENT_3D('',#15766,#12332,#12333);
#10178=AXIS2_PLACEMENT_3D('',#15767,#12334,#12335);
#10179=AXIS2_PLACEMENT_3D('',#15769,#12336,#12337);
#10180=AXIS2_PLACEMENT_3D('',#15770,#12338,#12339);
#10181=AXIS2_PLACEMENT_3D('',#15771,#12340,#12341);
#10182=AXIS2_PLACEMENT_3D('',#15795,#12342,#12343);
#10183=AXIS2_PLACEMENT_3D('',#15796,#12344,#12345);
#10184=AXIS2_PLACEMENT_3D('',#15798,#12346,#12347);
#10185=AXIS2_PLACEMENT_3D('',#15799,#12348,#12349);
#10186=AXIS2_PLACEMENT_3D('',#15800,#12350,#12351);
#10187=AXIS2_PLACEMENT_3D('',#15824,#12352,#12353);
#10188=AXIS2_PLACEMENT_3D('',#15825,#12354,#12355);
#10189=AXIS2_PLACEMENT_3D('',#15827,#12356,#12357);
#10190=AXIS2_PLACEMENT_3D('',#15828,#12358,#12359);
#10191=AXIS2_PLACEMENT_3D('',#15829,#12360,#12361);
#10192=AXIS2_PLACEMENT_3D('',#15844,#12362,#12363);
#10193=AXIS2_PLACEMENT_3D('',#15857,#12364,#12365);
#10194=AXIS2_PLACEMENT_3D('',#15859,#12366,#12367);
#10195=AXIS2_PLACEMENT_3D('',#15860,#12368,#12369);
#10196=AXIS2_PLACEMENT_3D('',#15861,#12370,#12371);
#10197=AXIS2_PLACEMENT_3D('',#15885,#12372,#12373);
#10198=AXIS2_PLACEMENT_3D('',#15886,#12374,#12375);
#10199=AXIS2_PLACEMENT_3D('',#15888,#12376,#12377);
#10200=AXIS2_PLACEMENT_3D('',#15889,#12378,#12379);
#10201=AXIS2_PLACEMENT_3D('',#15890,#12380,#12381);
#10202=AXIS2_PLACEMENT_3D('',#15914,#12382,#12383);
#10203=AXIS2_PLACEMENT_3D('',#15915,#12384,#12385);
#10204=AXIS2_PLACEMENT_3D('',#15917,#12386,#12387);
#10205=AXIS2_PLACEMENT_3D('',#15918,#12388,#12389);
#10206=AXIS2_PLACEMENT_3D('',#15919,#12390,#12391);
#10207=AXIS2_PLACEMENT_3D('',#15943,#12392,#12393);
#10208=AXIS2_PLACEMENT_3D('',#15944,#12394,#12395);
#10209=AXIS2_PLACEMENT_3D('',#15946,#12396,#12397);
#10210=AXIS2_PLACEMENT_3D('',#15949,#12399,#12400);
#10211=AXIS2_PLACEMENT_3D('',#15973,#12401,#12402);
#10212=AXIS2_PLACEMENT_3D('',#15974,#12403,#12404);
#10213=AXIS2_PLACEMENT_3D('',#15975,#12405,#12406);
#10214=AXIS2_PLACEMENT_3D('',#15976,#12407,#12408);
#10215=AXIS2_PLACEMENT_3D('',#15977,#12409,#12410);
#10216=AXIS2_PLACEMENT_3D('',#15978,#12411,#12412);
#10217=AXIS2_PLACEMENT_3D('',#15979,#12413,#12414);
#10218=AXIS2_PLACEMENT_3D('',#15980,#12415,#12416);
#10219=AXIS2_PLACEMENT_3D('',#15981,#12417,#12418);
#10220=AXIS2_PLACEMENT_3D('',#15983,#12419,#12420);
#10221=AXIS2_PLACEMENT_3D('',#15985,#12421,#12422);
#10222=AXIS2_PLACEMENT_3D('',#15986,#12423,#12424);
#10223=AXIS2_PLACEMENT_3D('',#15988,#12425,#12426);
#10224=AXIS2_PLACEMENT_3D('',#15990,#12428,#12429);
#10225=AXIS2_PLACEMENT_3D('',#15992,#12430,#12431);
#10226=AXIS2_PLACEMENT_3D('',#15993,#12432,#12433);
#10227=AXIS2_PLACEMENT_3D('',#15995,#12435,#12436);
#10228=AXIS2_PLACEMENT_3D('',#15997,#12437,#12438);
#10229=AXIS2_PLACEMENT_3D('',#15999,#12439,#12440);
#10230=AXIS2_PLACEMENT_3D('',#16000,#12441,#12442);
#10231=AXIS2_PLACEMENT_3D('',#16002,#12443,#12444);
#10232=AXIS2_PLACEMENT_3D('',#16004,#12446,#12447);
#10233=AXIS2_PLACEMENT_3D('',#16006,#12448,#12449);
#10234=AXIS2_PLACEMENT_3D('',#16007,#12450,#12451);
#10235=AXIS2_PLACEMENT_3D('',#16009,#12453,#12454);
#10236=AXIS2_PLACEMENT_3D('',#16010,#12455,#12456);
#10237=AXIS2_PLACEMENT_3D('',#16011,#12457,#12458);
#10238=AXIS2_PLACEMENT_3D('',#16012,#12459,#12460);
#10239=AXIS2_PLACEMENT_3D('',#16013,#12461,#12462);
#10240=AXIS2_PLACEMENT_3D('',#16014,#12463,#12464);
#10241=AXIS2_PLACEMENT_3D('',#16015,#12465,#12466);
#10242=AXIS2_PLACEMENT_3D('',#16016,#12467,#12468);
#10243=AXIS2_PLACEMENT_3D('',#16017,#12469,#12470);
#10244=AXIS2_PLACEMENT_3D('',#16018,#12471,#12472);
#10245=AXIS2_PLACEMENT_3D('',#16019,#12473,#12474);
#10246=AXIS2_PLACEMENT_3D('',#16020,#12475,#12476);
#10247=AXIS2_PLACEMENT_3D('',#16021,#12477,#12478);
#10248=AXIS2_PLACEMENT_3D('',#16022,#12479,#12480);
#10249=AXIS2_PLACEMENT_3D('',#16023,#12481,#12482);
#10250=AXIS2_PLACEMENT_3D('',#16025,#12483,#12484);
#10251=AXIS2_PLACEMENT_3D('',#16028,#12486,#12487);
#10252=AXIS2_PLACEMENT_3D('',#16029,#12488,#12489);
#10253=AXIS2_PLACEMENT_3D('',#16030,#12490,#12491);
#10254=AXIS2_PLACEMENT_3D('',#16032,#12492,#12493);
#10255=AXIS2_PLACEMENT_3D('',#16035,#12495,#12496);
#10256=AXIS2_PLACEMENT_3D('',#16036,#12497,#12498);
#10257=AXIS2_PLACEMENT_3D('',#16037,#12499,#12500);
#10258=AXIS2_PLACEMENT_3D('',#16046,#12505,#12506);
#10259=AXIS2_PLACEMENT_3D('',#16055,#12511,#12512);
#10260=AXIS2_PLACEMENT_3D('',#16058,#12515,#12516);
#10261=AXIS2_PLACEMENT_3D('',#16060,#12518,#12519);
#10262=AXIS2_PLACEMENT_3D('',#16062,#12520,#12521);
#10263=AXIS2_PLACEMENT_3D('',#16065,#12523,#12524);
#10264=AXIS2_PLACEMENT_3D('',#16066,#12525,#12526);
#10265=AXIS2_PLACEMENT_3D('',#16075,#12531,#12532);
#10266=AXIS2_PLACEMENT_3D('',#16081,#12536,#12537);
#10267=AXIS2_PLACEMENT_3D('',#16087,#12541,#12542);
#10268=AXIS2_PLACEMENT_3D('',#16089,#12544,#12545);
#10269=AXIS2_PLACEMENT_3D('',#16091,#12547,#12548);
#10270=AXIS2_PLACEMENT_3D('',#16093,#12549,#12550);
#10271=AXIS2_PLACEMENT_3D('',#16096,#12552,#12553);
#10272=AXIS2_PLACEMENT_3D('',#16097,#12554,#12555);
#10273=AXIS2_PLACEMENT_3D('',#16099,#12556,#12557);
#10274=AXIS2_PLACEMENT_3D('',#16102,#12559,#12560);
#10275=AXIS2_PLACEMENT_3D('',#16103,#12561,#12562);
#10276=AXIS2_PLACEMENT_3D('',#16105,#12563,#12564);
#10277=AXIS2_PLACEMENT_3D('',#16108,#12566,#12567);
#10278=AXIS2_PLACEMENT_3D('',#16109,#12568,#12569);
#10279=AXIS2_PLACEMENT_3D('',#16111,#12570,#12571);
#10280=AXIS2_PLACEMENT_3D('',#16114,#12573,#12574);
#10281=AXIS2_PLACEMENT_3D('',#16115,#12575,#12576);
#10282=AXIS2_PLACEMENT_3D('',#16124,#12581,#12582);
#10283=AXIS2_PLACEMENT_3D('',#16130,#12586,#12587);
#10284=AXIS2_PLACEMENT_3D('',#16137,#12592,#12593);
#10285=AXIS2_PLACEMENT_3D('',#16140,#12596,#12597);
#10286=AXIS2_PLACEMENT_3D('',#16141,#12598,#12599);
#10287=AXIS2_PLACEMENT_3D('',#16142,#12600,#12601);
#10288=AXIS2_PLACEMENT_3D('',#16143,#12602,#12603);
#10289=AXIS2_PLACEMENT_3D('',#16145,#12604,#12605);
#10290=AXIS2_PLACEMENT_3D('',#16148,#12607,#12608);
#10291=AXIS2_PLACEMENT_3D('',#16149,#12609,#12610);
#10292=AXIS2_PLACEMENT_3D('',#16151,#12611,#12612);
#10293=AXIS2_PLACEMENT_3D('',#16154,#12614,#12615);
#10294=AXIS2_PLACEMENT_3D('',#16155,#12616,#12617);
#10295=AXIS2_PLACEMENT_3D('',#16164,#12622,#12623);
#10296=AXIS2_PLACEMENT_3D('',#16170,#12627,#12628);
#10297=AXIS2_PLACEMENT_3D('',#16176,#12632,#12633);
#10298=AXIS2_PLACEMENT_3D('',#16179,#12636,#12637);
#10299=AXIS2_PLACEMENT_3D('',#16180,#12638,#12639);
#10300=AXIS2_PLACEMENT_3D('',#16181,#12640,#12641);
#10301=AXIS2_PLACEMENT_3D('',#16182,#12642,#12643);
#10302=AXIS2_PLACEMENT_3D('',#16184,#12644,#12645);
#10303=AXIS2_PLACEMENT_3D('',#16187,#12647,#12648);
#10304=AXIS2_PLACEMENT_3D('',#16188,#12649,#12650);
#10305=AXIS2_PLACEMENT_3D('',#16189,#12651,#12652);
#10306=AXIS2_PLACEMENT_3D('',#16191,#12653,#12654);
#10307=AXIS2_PLACEMENT_3D('',#16193,#12655,#12656);
#10308=AXIS2_PLACEMENT_3D('',#16194,#12657,#12658);
#10309=AXIS2_PLACEMENT_3D('',#16197,#12660,#12661);
#10310=AXIS2_PLACEMENT_3D('',#16198,#12662,#12663);
#10311=AXIS2_PLACEMENT_3D('',#16199,#12664,#12665);
#10312=AXIS2_PLACEMENT_3D('',#16201,#12666,#12667);
#10313=AXIS2_PLACEMENT_3D('',#16203,#12669,#12670);
#10314=AXIS2_PLACEMENT_3D('',#16204,#12671,#12672);
#10315=AXIS2_PLACEMENT_3D('',#16205,#12673,#12674);
#10316=AXIS2_PLACEMENT_3D('',#16207,#12675,#12676);
#10317=AXIS2_PLACEMENT_3D('',#16210,#12678,#12679);
#10318=AXIS2_PLACEMENT_3D('',#16211,#12680,#12681);
#10319=AXIS2_PLACEMENT_3D('',#16213,#12682,#12683);
#10320=AXIS2_PLACEMENT_3D('',#16216,#12685,#12686);
#10321=AXIS2_PLACEMENT_3D('',#16217,#12687,#12688);
#10322=AXIS2_PLACEMENT_3D('',#16218,#12689,#12690);
#10323=AXIS2_PLACEMENT_3D('',#16219,#12691,#12692);
#10324=AXIS2_PLACEMENT_3D('',#16220,#12693,#12694);
#10325=AXIS2_PLACEMENT_3D('',#16222,#12695,#12696);
#10326=AXIS2_PLACEMENT_3D('',#16225,#12698,#12699);
#10327=AXIS2_PLACEMENT_3D('',#16226,#12700,#12701);
#10328=AXIS2_PLACEMENT_3D('',#16228,#12702,#12703);
#10329=AXIS2_PLACEMENT_3D('',#16231,#12705,#12706);
#10330=AXIS2_PLACEMENT_3D('',#16232,#12707,#12708);
#10331=AXIS2_PLACEMENT_3D('',#16233,#12709,#12710);
#10332=AXIS2_PLACEMENT_3D('',#16234,#12711,#12712);
#10333=AXIS2_PLACEMENT_3D('',#16235,#12713,#12714);
#10334=AXIS2_PLACEMENT_3D('',#16237,#12715,#12716);
#10335=AXIS2_PLACEMENT_3D('',#16240,#12718,#12719);
#10336=AXIS2_PLACEMENT_3D('',#16241,#12720,#12721);
#10337=AXIS2_PLACEMENT_3D('',#16243,#12722,#12723);
#10338=AXIS2_PLACEMENT_3D('',#16246,#12725,#12726);
#10339=AXIS2_PLACEMENT_3D('',#16247,#12727,#12728);
#10340=AXIS2_PLACEMENT_3D('',#16248,#12729,#12730);
#10341=AXIS2_PLACEMENT_3D('',#16249,#12731,#12732);
#10342=AXIS2_PLACEMENT_3D('',#16250,#12733,#12734);
#10343=AXIS2_PLACEMENT_3D('',#16251,#12735,#12736);
#10344=AXIS2_PLACEMENT_3D('',#16255,#12738,#12739);
#10345=AXIS2_PLACEMENT_3D('',#16256,#12740,#12741);
#10346=AXIS2_PLACEMENT_3D('',#16260,#12743,#12744);
#10347=AXIS2_PLACEMENT_3D('',#16263,#12746,#12747);
#10348=AXIS2_PLACEMENT_3D('',#16265,#12748,#12749);
#10349=AXIS2_PLACEMENT_3D('',#16267,#12751,#12752);
#10350=AXIS2_PLACEMENT_3D('',#16271,#12754,#12755);
#10351=AXIS2_PLACEMENT_3D('',#16272,#12756,#12757);
#10352=AXIS2_PLACEMENT_3D('',#16276,#12759,#12760);
#10353=AXIS2_PLACEMENT_3D('',#16279,#12762,#12763);
#10354=AXIS2_PLACEMENT_3D('',#16281,#12764,#12765);
#10355=AXIS2_PLACEMENT_3D('',#16283,#12767,#12768);
#10356=AXIS2_PLACEMENT_3D('',#16287,#12770,#12771);
#10357=AXIS2_PLACEMENT_3D('',#16288,#12772,#12773);
#10358=AXIS2_PLACEMENT_3D('',#16292,#12775,#12776);
#10359=AXIS2_PLACEMENT_3D('',#16295,#12778,#12779);
#10360=AXIS2_PLACEMENT_3D('',#16297,#12780,#12781);
#10361=AXIS2_PLACEMENT_3D('',#16299,#12783,#12784);
#10362=AXIS2_PLACEMENT_3D('',#16303,#12786,#12787);
#10363=AXIS2_PLACEMENT_3D('',#16304,#12788,#12789);
#10364=AXIS2_PLACEMENT_3D('',#16308,#12791,#12792);
#10365=AXIS2_PLACEMENT_3D('',#16311,#12794,#12795);
#10366=AXIS2_PLACEMENT_3D('',#16313,#12796,#12797);
#10367=AXIS2_PLACEMENT_3D('',#16315,#12799,#12800);
#10368=AXIS2_PLACEMENT_3D('',#16326,#12807,#12808);
#10369=AXIS2_PLACEMENT_3D('',#16337,#12815,#12816);
#10370=AXIS2_PLACEMENT_3D('',#16356,#12827,#12828);
#10371=AXIS2_PLACEMENT_3D('',#16360,#12831,#12832);
#10372=AXIS2_PLACEMENT_3D('',#16364,#12835,#12836);
#10373=AXIS2_PLACEMENT_3D('',#16368,#12839,#12840);
#10374=AXIS2_PLACEMENT_3D('',#16372,#12843,#12844);
#10375=AXIS2_PLACEMENT_3D('',#16374,#12846,#12847);
#10376=AXIS2_PLACEMENT_3D('',#16378,#12850,#12851);
#10377=AXIS2_PLACEMENT_3D('',#16382,#12854,#12855);
#10378=AXIS2_PLACEMENT_3D('',#16386,#12858,#12859);
#10379=AXIS2_PLACEMENT_3D('',#16390,#12862,#12863);
#10380=AXIS2_PLACEMENT_3D('',#16392,#12865,#12866);
#10381=AXIS2_PLACEMENT_3D('',#16393,#12867,#12868);
#10382=AXIS2_PLACEMENT_3D('',#16394,#12869,#12870);
#10383=AXIS2_PLACEMENT_3D('',#16403,#12875,#12876);
#10384=AXIS2_PLACEMENT_3D('',#16409,#12880,#12881);
#10385=AXIS2_PLACEMENT_3D('',#16415,#12885,#12886);
#10386=AXIS2_PLACEMENT_3D('',#16421,#12890,#12891);
#10387=AXIS2_PLACEMENT_3D('',#16427,#12895,#12896);
#10388=AXIS2_PLACEMENT_3D('',#16433,#12900,#12901);
#10389=AXIS2_PLACEMENT_3D('',#16439,#12905,#12906);
#10390=AXIS2_PLACEMENT_3D('',#16442,#12909,#12910);
#10391=AXIS2_PLACEMENT_3D('',#16443,#12911,#12912);
#10392=AXIS2_PLACEMENT_3D('',#16444,#12913,#12914);
#10393=AXIS2_PLACEMENT_3D('',#16445,#12915,#12916);
#10394=AXIS2_PLACEMENT_3D('',#16454,#12921,#12922);
#10395=AXIS2_PLACEMENT_3D('',#16460,#12926,#12927);
#10396=AXIS2_PLACEMENT_3D('',#16466,#12931,#12932);
#10397=AXIS2_PLACEMENT_3D('',#16472,#12936,#12937);
#10398=AXIS2_PLACEMENT_3D('',#16478,#12941,#12942);
#10399=AXIS2_PLACEMENT_3D('',#16484,#12946,#12947);
#10400=AXIS2_PLACEMENT_3D('',#16490,#12951,#12952);
#10401=AXIS2_PLACEMENT_3D('',#16493,#12955,#12956);
#10402=AXIS2_PLACEMENT_3D('',#16494,#12957,#12958);
#10403=AXIS2_PLACEMENT_3D('',#16495,#12959,#12960);
#10404=AXIS2_PLACEMENT_3D('',#16496,#12961,#12962);
#10405=AXIS2_PLACEMENT_3D('',#16497,#12963,#12964);
#10406=AXIS2_PLACEMENT_3D('',#16498,#12965,#12966);
#10407=AXIS2_PLACEMENT_3D('',#16499,#12967,#12968);
#10408=AXIS2_PLACEMENT_3D('',#16508,#12973,#12974);
#10409=AXIS2_PLACEMENT_3D('',#16514,#12978,#12979);
#10410=AXIS2_PLACEMENT_3D('',#16520,#12983,#12984);
#10411=AXIS2_PLACEMENT_3D('',#16526,#12988,#12989);
#10412=AXIS2_PLACEMENT_3D('',#16532,#12993,#12994);
#10413=AXIS2_PLACEMENT_3D('',#16535,#12997,#12998);
#10414=AXIS2_PLACEMENT_3D('',#16536,#12999,#13000);
#10415=AXIS2_PLACEMENT_3D('',#16537,#13001,#13002);
#10416=AXIS2_PLACEMENT_3D('',#16539,#13003,#13004);
#10417=AXIS2_PLACEMENT_3D('',#16540,#13005,#13006);
#10418=AXIS2_PLACEMENT_3D('',#16542,#13007,#13008);
#10419=AXIS2_PLACEMENT_3D('',#16543,#13009,#13010);
#10420=AXIS2_PLACEMENT_3D('',#16545,#13011,#13012);
#10421=AXIS2_PLACEMENT_3D('',#16547,#13014,#13015);
#10422=AXIS2_PLACEMENT_3D('',#16549,#13016,#13017);
#10423=AXIS2_PLACEMENT_3D('',#16551,#13019,#13020);
#10424=AXIS2_PLACEMENT_3D('',#16553,#13021,#13022);
#10425=AXIS2_PLACEMENT_3D('',#16555,#13024,#13025);
#10426=AXIS2_PLACEMENT_3D('',#16557,#13026,#13027);
#10427=AXIS2_PLACEMENT_3D('',#16558,#13028,#13029);
#10428=AXIS2_PLACEMENT_3D('',#16560,#13030,#13031);
#10429=AXIS2_PLACEMENT_3D('',#16562,#13033,#13034);
#10430=AXIS2_PLACEMENT_3D('',#16564,#13036,#13037);
#10431=AXIS2_PLACEMENT_3D('',#16565,#13038,#13039);
#10432=AXIS2_PLACEMENT_3D('',#16567,#13040,#13041);
#10433=AXIS2_PLACEMENT_3D('',#16570,#13043,#13044);
#10434=AXIS2_PLACEMENT_3D('',#16571,#13045,#13046);
#10435=AXIS2_PLACEMENT_3D('',#16574,#13048,#13049);
#10436=AXIS2_PLACEMENT_3D('',#16575,#13050,#13051);
#10437=AXIS2_PLACEMENT_3D('',#16577,#13052,#13053);
#10438=AXIS2_PLACEMENT_3D('',#16578,#13054,#13055);
#10439=AXIS2_PLACEMENT_3D('',#16581,#13057,#13058);
#10440=AXIS2_PLACEMENT_3D('',#16582,#13059,#13060);
#10441=AXIS2_PLACEMENT_3D('',#16583,#13061,#13062);
#10442=AXIS2_PLACEMENT_3D('',#16584,#13063,#13064);
#10443=AXIS2_PLACEMENT_3D('',#16586,#13065,#13066);
#10444=AXIS2_PLACEMENT_3D('',#16587,#13067,#13068);
#10445=AXIS2_PLACEMENT_3D('',#16589,#13069,#13070);
#10446=AXIS2_PLACEMENT_3D('',#16591,#13072,#13073);
#10447=AXIS2_PLACEMENT_3D('',#16593,#13074,#13075);
#10448=AXIS2_PLACEMENT_3D('',#16595,#13077,#13078);
#10449=AXIS2_PLACEMENT_3D('',#16597,#13079,#13080);
#10450=AXIS2_PLACEMENT_3D('',#16599,#13082,#13083);
#10451=AXIS2_PLACEMENT_3D('',#16601,#13084,#13085);
#10452=AXIS2_PLACEMENT_3D('',#16602,#13086,#13087);
#10453=AXIS2_PLACEMENT_3D('',#16604,#13088,#13089);
#10454=AXIS2_PLACEMENT_3D('',#16606,#13091,#13092);
#10455=AXIS2_PLACEMENT_3D('',#16608,#13093,#13094);
#10456=AXIS2_PLACEMENT_3D('',#16610,#13096,#13097);
#10457=AXIS2_PLACEMENT_3D('',#16612,#13098,#13099);
#10458=AXIS2_PLACEMENT_3D('',#16614,#13101,#13102);
#10459=AXIS2_PLACEMENT_3D('',#16615,#13103,#13104);
#10460=AXIS2_PLACEMENT_3D('',#16624,#13109,#13110);
#10461=AXIS2_PLACEMENT_3D('',#16630,#13114,#13115);
#10462=AXIS2_PLACEMENT_3D('',#16636,#13119,#13120);
#10463=AXIS2_PLACEMENT_3D('',#16642,#13124,#13125);
#10464=AXIS2_PLACEMENT_3D('',#16648,#13129,#13130);
#10465=AXIS2_PLACEMENT_3D('',#16651,#13133,#13134);
#10466=AXIS2_PLACEMENT_3D('',#16652,#13135,#13136);
#10467=AXIS2_PLACEMENT_3D('',#16653,#13137,#13138);
#10468=AXIS2_PLACEMENT_3D('',#16654,#13139,#13140);
#10469=AXIS2_PLACEMENT_3D('',#16655,#13141,#13142);
#10470=AXIS2_PLACEMENT_3D('',#16656,#13143,#13144);
#10471=AXIS2_PLACEMENT_3D('',#16657,#13145,#13146);
#10472=AXIS2_PLACEMENT_3D('',#16658,#13147,#13148);
#10473=AXIS2_PLACEMENT_3D('',#16659,#13149,#13150);
#10474=AXIS2_PLACEMENT_3D('',#16660,#13151,#13152);
#10475=AXIS2_PLACEMENT_3D('',#16661,#13153,#13154);
#10476=AXIS2_PLACEMENT_3D('',#16662,#13155,#13156);
#10477=AXIS2_PLACEMENT_3D('',#16663,#13157,#13158);
#10478=AXIS2_PLACEMENT_3D('',#16664,#13159,#13160);
#10479=AXIS2_PLACEMENT_3D('',#16665,#13161,#13162);
#10480=AXIS2_PLACEMENT_3D('',#16666,#13163,#13164);
#10481=AXIS2_PLACEMENT_3D('',#16667,#13165,#13166);
#10482=AXIS2_PLACEMENT_3D('',#16668,#13167,#13168);
#10483=AXIS2_PLACEMENT_3D('',#16669,#13169,#13170);
#10484=AXIS2_PLACEMENT_3D('',#16670,#13171,#13172);
#10485=AXIS2_PLACEMENT_3D('',#16671,#13173,#13174);
#10486=AXIS2_PLACEMENT_3D('',#16672,#13175,#13176);
#10487=AXIS2_PLACEMENT_3D('',#16673,#13177,#13178);
#10488=AXIS2_PLACEMENT_3D('',#16674,#13179,#13180);
#10489=AXIS2_PLACEMENT_3D('',#16675,#13181,#13182);
#10490=AXIS2_PLACEMENT_3D('',#16676,#13183,#13184);
#10491=AXIS2_PLACEMENT_3D('',#16677,#13185,#13186);
#10492=AXIS2_PLACEMENT_3D('',#16678,#13187,#13188);
#10493=AXIS2_PLACEMENT_3D('',#16679,#13189,#13190);
#10494=AXIS2_PLACEMENT_3D('',#16680,#13191,#13192);
#10495=AXIS2_PLACEMENT_3D('',#16681,#13193,#13194);
#10496=AXIS2_PLACEMENT_3D('',#16682,#13195,#13196);
#10497=AXIS2_PLACEMENT_3D('',#16683,#13197,#13198);
#10498=AXIS2_PLACEMENT_3D('',#16684,#13199,#13200);
#10499=AXIS2_PLACEMENT_3D('',#16685,#13201,#13202);
#10500=AXIS2_PLACEMENT_3D('',#16686,#13203,#13204);
#10501=AXIS2_PLACEMENT_3D('',#16687,#13205,#13206);
#10502=AXIS2_PLACEMENT_3D('',#16688,#13207,#13208);
#10503=AXIS2_PLACEMENT_3D('',#16689,#13209,#13210);
#10504=AXIS2_PLACEMENT_3D('',#16690,#13211,#13212);
#10505=AXIS2_PLACEMENT_3D('',#16691,#13213,#13214);
#10506=AXIS2_PLACEMENT_3D('',#16700,#13219,#13220);
#10507=AXIS2_PLACEMENT_3D('',#16706,#13224,#13225);
#10508=AXIS2_PLACEMENT_3D('',#16712,#13229,#13230);
#10509=AXIS2_PLACEMENT_3D('',#16718,#13234,#13235);
#10510=AXIS2_PLACEMENT_3D('',#16724,#13239,#13240);
#10511=AXIS2_PLACEMENT_3D('',#16727,#13243,#13244);
#10512=AXIS2_PLACEMENT_3D('',#16728,#13245,#13246);
#10513=AXIS2_PLACEMENT_3D('',#16729,#13247,#13248);
#10514=AXIS2_PLACEMENT_3D('',#16731,#13249,#13250);
#10515=AXIS2_PLACEMENT_3D('',#16732,#13251,#13252);
#10516=AXIS2_PLACEMENT_3D('',#16734,#13253,#13254);
#10517=AXIS2_PLACEMENT_3D('',#16735,#13255,#13256);
#10518=AXIS2_PLACEMENT_3D('',#16737,#13257,#13258);
#10519=AXIS2_PLACEMENT_3D('',#16739,#13260,#13261);
#10520=AXIS2_PLACEMENT_3D('',#16741,#13262,#13263);
#10521=AXIS2_PLACEMENT_3D('',#16743,#13265,#13266);
#10522=AXIS2_PLACEMENT_3D('',#16745,#13267,#13268);
#10523=AXIS2_PLACEMENT_3D('',#16747,#13270,#13271);
#10524=AXIS2_PLACEMENT_3D('',#16749,#13272,#13273);
#10525=AXIS2_PLACEMENT_3D('',#16750,#13274,#13275);
#10526=AXIS2_PLACEMENT_3D('',#16752,#13276,#13277);
#10527=AXIS2_PLACEMENT_3D('',#16754,#13279,#13280);
#10528=AXIS2_PLACEMENT_3D('',#16756,#13282,#13283);
#10529=AXIS2_PLACEMENT_3D('',#16757,#13284,#13285);
#10530=AXIS2_PLACEMENT_3D('',#16758,#13286,#13287);
#10531=AXIS2_PLACEMENT_3D('',#16759,#13288,#13289);
#10532=AXIS2_PLACEMENT_3D('',#16760,#13290,#13291);
#10533=AXIS2_PLACEMENT_3D('',#16761,#13292,#13293);
#10534=AXIS2_PLACEMENT_3D('',#16762,#13294,#13295);
#10535=AXIS2_PLACEMENT_3D('',#16763,#13296,#13297);
#10536=AXIS2_PLACEMENT_3D('',#16764,#13298,#13299);
#10537=AXIS2_PLACEMENT_3D('',#16765,#13300,#13301);
#10538=AXIS2_PLACEMENT_3D('',#16766,#13302,#13303);
#10539=AXIS2_PLACEMENT_3D('',#16767,#13304,#13305);
#10540=AXIS2_PLACEMENT_3D('',#16768,#13306,#13307);
#10541=AXIS2_PLACEMENT_3D('',#16769,#13308,#13309);
#10542=AXIS2_PLACEMENT_3D('',#16770,#13310,#13311);
#10543=AXIS2_PLACEMENT_3D('',#16771,#13312,#13313);
#10544=AXIS2_PLACEMENT_3D('',#16772,#13314,#13315);
#10545=AXIS2_PLACEMENT_3D('',#16773,#13316,#13317);
#10546=AXIS2_PLACEMENT_3D('',#16774,#13318,#13319);
#10547=AXIS2_PLACEMENT_3D('',#16775,#13320,#13321);
#10548=AXIS2_PLACEMENT_3D('',#16776,#13322,#13323);
#10549=AXIS2_PLACEMENT_3D('',#16777,#13324,#13325);
#10550=AXIS2_PLACEMENT_3D('',#16778,#13326,#13327);
#10551=AXIS2_PLACEMENT_3D('',#16779,#13328,#13329);
#10552=AXIS2_PLACEMENT_3D('',#16780,#13330,#13331);
#10553=AXIS2_PLACEMENT_3D('',#16781,#13332,#13333);
#10554=AXIS2_PLACEMENT_3D('',#16782,#13334,#13335);
#10555=AXIS2_PLACEMENT_3D('',#16783,#13336,#13337);
#10556=AXIS2_PLACEMENT_3D('',#16784,#13338,#13339);
#10557=AXIS2_PLACEMENT_3D('',#16785,#13340,#13341);
#10558=AXIS2_PLACEMENT_3D('',#16786,#13342,#13343);
#10559=AXIS2_PLACEMENT_3D('',#16787,#13344,#13345);
#10560=AXIS2_PLACEMENT_3D('',#16788,#13346,#13347);
#10561=AXIS2_PLACEMENT_3D('',#16789,#13348,#13349);
#10562=AXIS2_PLACEMENT_3D('',#16790,#13350,#13351);
#10563=AXIS2_PLACEMENT_3D('',#16791,#13352,#13353);
#10564=AXIS2_PLACEMENT_3D('',#16792,#13354,#13355);
#10565=AXIS2_PLACEMENT_3D('',#16793,#13356,#13357);
#10566=DIRECTION('axis',(0.,0.,1.));
#10567=DIRECTION('refdir',(1.,0.,0.));
#10568=DIRECTION('axis',(0.,0.,1.));
#10569=DIRECTION('refdir',(1.,0.,0.));
#10570=DIRECTION('axis',(0.,0.,1.));
#10571=DIRECTION('refdir',(1.,0.,0.));
#10572=DIRECTION('center_axis',(0.,0.,1.));
#10573=DIRECTION('ref_axis',(1.,0.,0.));
#10574=DIRECTION('center_axis',(0.,0.,1.));
#10575=DIRECTION('ref_axis',(1.,0.,0.));
#10576=DIRECTION('',(0.,0.,1.));
#10577=DIRECTION('center_axis',(0.,0.,-1.));
#10578=DIRECTION('ref_axis',(1.,0.,0.));
#10579=DIRECTION('center_axis',(0.,0.,1.));
#10580=DIRECTION('ref_axis',(1.,0.,0.));
#10581=DIRECTION('center_axis',(0.,0.,1.));
#10582=DIRECTION('ref_axis',(1.,0.,0.));
#10583=DIRECTION('',(0.,0.,1.));
#10584=DIRECTION('center_axis',(0.,0.,-1.));
#10585=DIRECTION('ref_axis',(1.,0.,0.));
#10586=DIRECTION('center_axis',(0.,0.,1.));
#10587=DIRECTION('ref_axis',(1.,0.,0.));
#10588=DIRECTION('center_axis',(0.,0.,1.));
#10589=DIRECTION('ref_axis',(1.,0.,0.));
#10590=DIRECTION('',(0.,0.,1.));
#10591=DIRECTION('center_axis',(0.,0.,-1.));
#10592=DIRECTION('ref_axis',(1.,0.,0.));
#10593=DIRECTION('center_axis',(0.,0.,1.));
#10594=DIRECTION('ref_axis',(1.,0.,0.));
#10595=DIRECTION('center_axis',(0.,0.,1.));
#10596=DIRECTION('ref_axis',(1.,0.,0.));
#10597=DIRECTION('',(0.,0.,1.));
#10598=DIRECTION('center_axis',(0.,0.,-1.));
#10599=DIRECTION('ref_axis',(1.,0.,0.));
#10600=DIRECTION('center_axis',(0.,0.,1.));
#10601=DIRECTION('ref_axis',(1.,0.,0.));
#10602=DIRECTION('center_axis',(0.,0.,1.));
#10603=DIRECTION('ref_axis',(1.,0.,0.));
#10604=DIRECTION('',(0.,0.,1.));
#10605=DIRECTION('center_axis',(0.,0.,-1.));
#10606=DIRECTION('ref_axis',(1.,0.,0.));
#10607=DIRECTION('center_axis',(0.,0.,1.));
#10608=DIRECTION('ref_axis',(1.,0.,0.));
#10609=DIRECTION('center_axis',(0.,0.,1.));
#10610=DIRECTION('ref_axis',(1.,0.,0.));
#10611=DIRECTION('',(0.,0.,1.));
#10612=DIRECTION('center_axis',(0.,0.,-1.));
#10613=DIRECTION('ref_axis',(1.,0.,0.));
#10614=DIRECTION('center_axis',(0.,0.,1.));
#10615=DIRECTION('ref_axis',(1.,0.,0.));
#10616=DIRECTION('center_axis',(0.,0.,1.));
#10617=DIRECTION('ref_axis',(1.,0.,0.));
#10618=DIRECTION('',(0.,0.,1.));
#10619=DIRECTION('center_axis',(0.,0.,-1.));
#10620=DIRECTION('ref_axis',(1.,0.,0.));
#10621=DIRECTION('center_axis',(0.,0.,1.));
#10622=DIRECTION('ref_axis',(1.,0.,0.));
#10623=DIRECTION('center_axis',(0.,0.,1.));
#10624=DIRECTION('ref_axis',(1.,0.,0.));
#10625=DIRECTION('',(0.,0.,1.));
#10626=DIRECTION('center_axis',(0.,0.,-1.));
#10627=DIRECTION('ref_axis',(1.,0.,0.));
#10628=DIRECTION('center_axis',(0.,0.,1.));
#10629=DIRECTION('ref_axis',(1.,0.,0.));
#10630=DIRECTION('center_axis',(0.,0.,1.));
#10631=DIRECTION('ref_axis',(1.,0.,0.));
#10632=DIRECTION('',(0.,0.,1.));
#10633=DIRECTION('center_axis',(0.,0.,-1.));
#10634=DIRECTION('ref_axis',(1.,0.,0.));
#10635=DIRECTION('center_axis',(0.,0.,1.));
#10636=DIRECTION('ref_axis',(1.,0.,0.));
#10637=DIRECTION('center_axis',(0.,0.,1.));
#10638=DIRECTION('ref_axis',(1.,0.,0.));
#10639=DIRECTION('',(0.,0.,1.));
#10640=DIRECTION('center_axis',(0.,0.,-1.));
#10641=DIRECTION('ref_axis',(1.,0.,0.));
#10642=DIRECTION('center_axis',(0.,0.,1.));
#10643=DIRECTION('ref_axis',(1.,0.,0.));
#10644=DIRECTION('center_axis',(0.,0.,1.));
#10645=DIRECTION('ref_axis',(1.,0.,0.));
#10646=DIRECTION('',(0.,0.,1.));
#10647=DIRECTION('center_axis',(0.,0.,-1.));
#10648=DIRECTION('ref_axis',(1.,0.,0.));
#10649=DIRECTION('center_axis',(0.,0.,1.));
#10650=DIRECTION('ref_axis',(1.,0.,0.));
#10651=DIRECTION('center_axis',(0.,0.,1.));
#10652=DIRECTION('ref_axis',(1.,0.,0.));
#10653=DIRECTION('',(0.,0.,1.));
#10654=DIRECTION('center_axis',(0.,0.,-1.));
#10655=DIRECTION('ref_axis',(1.,0.,0.));
#10656=DIRECTION('center_axis',(0.,1.,0.));
#10657=DIRECTION('ref_axis',(-1.,0.,0.));
#10658=DIRECTION('',(-1.,0.,0.));
#10659=DIRECTION('',(0.,0.,1.));
#10660=DIRECTION('',(-1.,0.,0.));
#10661=DIRECTION('',(0.,0.,1.));
#10662=DIRECTION('center_axis',(1.,0.,0.));
#10663=DIRECTION('ref_axis',(0.,1.,0.));
#10664=DIRECTION('',(0.,1.,0.));
#10665=DIRECTION('',(0.,1.,0.));
#10666=DIRECTION('',(0.,0.,1.));
#10667=DIRECTION('center_axis',(0.,-1.,0.));
#10668=DIRECTION('ref_axis',(1.,0.,0.));
#10669=DIRECTION('',(1.,0.,0.));
#10670=DIRECTION('',(1.,0.,0.));
#10671=DIRECTION('',(0.,0.,1.));
#10672=DIRECTION('center_axis',(-1.,0.,0.));
#10673=DIRECTION('ref_axis',(0.,-1.,0.));
#10674=DIRECTION('',(0.,-1.,0.));
#10675=DIRECTION('',(0.,-1.,0.));
#10676=DIRECTION('center_axis',(0.,0.,1.));
#10677=DIRECTION('ref_axis',(1.,0.,0.));
#10678=DIRECTION('center_axis',(0.,0.,1.));
#10679=DIRECTION('ref_axis',(1.,0.,0.));
#10680=DIRECTION('axis',(0.,0.,1.));
#10681=DIRECTION('refdir',(1.,0.,0.));
#10682=DIRECTION('center_axis',(0.,0.,1.));
#10683=DIRECTION('ref_axis',(1.,0.,0.));
#10684=DIRECTION('center_axis',(0.,0.,1.));
#10685=DIRECTION('ref_axis',(1.,0.,0.));
#10686=DIRECTION('',(0.,0.,1.));
#10687=DIRECTION('center_axis',(0.,0.,-1.));
#10688=DIRECTION('ref_axis',(1.,0.,0.));
#10689=DIRECTION('center_axis',(0.,0.,1.));
#10690=DIRECTION('ref_axis',(1.,0.,0.));
#10691=DIRECTION('center_axis',(0.,0.,1.));
#10692=DIRECTION('ref_axis',(1.,0.,0.));
#10693=DIRECTION('center_axis',(0.,0.,1.));
#10694=DIRECTION('ref_axis',(1.,0.,0.));
#10695=DIRECTION('',(0.,0.,1.));
#10696=DIRECTION('center_axis',(0.,0.,-1.));
#10697=DIRECTION('ref_axis',(1.,0.,0.));
#10698=DIRECTION('center_axis',(0.,0.,1.));
#10699=DIRECTION('ref_axis',(1.,0.,0.));
#10700=DIRECTION('center_axis',(0.,0.,1.));
#10701=DIRECTION('ref_axis',(1.,0.,0.));
#10702=DIRECTION('center_axis',(0.,0.,1.));
#10703=DIRECTION('ref_axis',(1.,0.,0.));
#10704=DIRECTION('',(0.,0.,1.));
#10705=DIRECTION('center_axis',(0.,0.,-1.));
#10706=DIRECTION('ref_axis',(1.,0.,0.));
#10707=DIRECTION('center_axis',(0.,0.,1.));
#10708=DIRECTION('ref_axis',(1.,0.,0.));
#10709=DIRECTION('center_axis',(0.,0.,1.));
#10710=DIRECTION('ref_axis',(1.,0.,0.));
#10711=DIRECTION('center_axis',(0.,0.,1.));
#10712=DIRECTION('ref_axis',(1.,0.,0.));
#10713=DIRECTION('center_axis',(0.,0.,1.));
#10714=DIRECTION('ref_axis',(1.,0.,0.));
#10715=DIRECTION('',(0.,0.,1.));
#10716=DIRECTION('center_axis',(0.,0.,-1.));
#10717=DIRECTION('ref_axis',(1.,0.,0.));
#10718=DIRECTION('center_axis',(0.,0.,1.));
#10719=DIRECTION('ref_axis',(1.,0.,0.));
#10720=DIRECTION('center_axis',(0.,0.,1.));
#10721=DIRECTION('ref_axis',(1.,0.,0.));
#10722=DIRECTION('center_axis',(0.,0.,1.));
#10723=DIRECTION('ref_axis',(1.,0.,0.));
#10724=DIRECTION('center_axis',(0.,0.,1.));
#10725=DIRECTION('ref_axis',(1.,0.,0.));
#10726=DIRECTION('',(0.,0.,1.));
#10727=DIRECTION('center_axis',(0.,0.,-1.));
#10728=DIRECTION('ref_axis',(1.,0.,0.));
#10729=DIRECTION('center_axis',(0.,0.,1.));
#10730=DIRECTION('ref_axis',(1.,0.,0.));
#10731=DIRECTION('center_axis',(0.,0.,1.));
#10732=DIRECTION('ref_axis',(1.,0.,0.));
#10733=DIRECTION('center_axis',(0.,0.,1.));
#10734=DIRECTION('ref_axis',(1.,0.,0.));
#10735=DIRECTION('center_axis',(0.,0.,1.));
#10736=DIRECTION('ref_axis',(1.,0.,0.));
#10737=DIRECTION('',(0.,0.,1.));
#10738=DIRECTION('center_axis',(0.,0.,-1.));
#10739=DIRECTION('ref_axis',(1.,0.,0.));
#10740=DIRECTION('center_axis',(0.,0.,1.));
#10741=DIRECTION('ref_axis',(1.,0.,0.));
#10742=DIRECTION('center_axis',(0.,0.,1.));
#10743=DIRECTION('ref_axis',(1.,0.,0.));
#10744=DIRECTION('center_axis',(0.,0.,1.));
#10745=DIRECTION('ref_axis',(1.,0.,0.));
#10746=DIRECTION('center_axis',(0.,0.,1.));
#10747=DIRECTION('ref_axis',(1.,0.,0.));
#10748=DIRECTION('',(0.,0.,1.));
#10749=DIRECTION('center_axis',(0.,0.,1.));
#10750=DIRECTION('ref_axis',(1.,0.,0.));
#10751=DIRECTION('center_axis',(0.,0.,1.));
#10752=DIRECTION('ref_axis',(1.,0.,0.));
#10753=DIRECTION('',(0.,0.,1.));
#10754=DIRECTION('center_axis',(0.,0.,1.));
#10755=DIRECTION('ref_axis',(1.,0.,0.));
#10756=DIRECTION('center_axis',(0.,0.,1.));
#10757=DIRECTION('ref_axis',(1.,0.,0.));
#10758=DIRECTION('',(0.,0.,1.));
#10759=DIRECTION('center_axis',(0.,0.,1.));
#10760=DIRECTION('ref_axis',(1.,0.,0.));
#10761=DIRECTION('center_axis',(0.,0.,1.));
#10762=DIRECTION('ref_axis',(1.,0.,0.));
#10763=DIRECTION('',(0.,0.,1.));
#10764=DIRECTION('center_axis',(0.,1.,0.));
#10765=DIRECTION('ref_axis',(-1.,0.,0.));
#10766=DIRECTION('',(-1.,0.,0.));
#10767=DIRECTION('',(0.,0.,1.));
#10768=DIRECTION('',(-1.,0.,0.));
#10769=DIRECTION('',(0.,0.,1.));
#10770=DIRECTION('center_axis',(1.,0.,0.));
#10771=DIRECTION('ref_axis',(0.,1.,0.));
#10772=DIRECTION('',(0.,1.,0.));
#10773=DIRECTION('',(0.,1.,0.));
#10774=DIRECTION('',(0.,0.,1.));
#10775=DIRECTION('center_axis',(0.,-1.,0.));
#10776=DIRECTION('ref_axis',(1.,0.,0.));
#10777=DIRECTION('',(1.,0.,0.));
#10778=DIRECTION('',(1.,0.,0.));
#10779=DIRECTION('',(0.,0.,1.));
#10780=DIRECTION('center_axis',(-1.,0.,0.));
#10781=DIRECTION('ref_axis',(0.,-1.,0.));
#10782=DIRECTION('',(0.,-1.,0.));
#10783=DIRECTION('',(0.,-1.,0.));
#10784=DIRECTION('center_axis',(0.,0.,1.));
#10785=DIRECTION('ref_axis',(1.,0.,0.));
#10786=DIRECTION('center_axis',(0.,0.,1.));
#10787=DIRECTION('ref_axis',(1.,0.,0.));
#10788=DIRECTION('axis',(0.,0.,1.));
#10789=DIRECTION('refdir',(1.,0.,0.));
#10790=DIRECTION('center_axis',(0.,0.,1.));
#10791=DIRECTION('ref_axis',(1.,0.,0.));
#10792=DIRECTION('center_axis',(0.,0.,-1.));
#10793=DIRECTION('ref_axis',(1.,0.,0.));
#10794=DIRECTION('',(0.,0.,-1.));
#10795=DIRECTION('center_axis',(0.,0.,-1.));
#10796=DIRECTION('ref_axis',(1.,0.,0.));
#10797=DIRECTION('center_axis',(0.,0.,1.));
#10798=DIRECTION('ref_axis',(1.,0.,0.));
#10799=DIRECTION('center_axis',(0.,0.,1.));
#10800=DIRECTION('ref_axis',(1.,0.,0.));
#10801=DIRECTION('',(0.,0.,-1.));
#10802=DIRECTION('center_axis',(0.,0.,1.));
#10803=DIRECTION('ref_axis',(1.,0.,0.));
#10804=DIRECTION('center_axis',(0.,0.,1.));
#10805=DIRECTION('ref_axis',(1.,0.,0.));
#10806=DIRECTION('center_axis',(0.,0.,1.));
#10807=DIRECTION('ref_axis',(1.,0.,0.));
#10808=DIRECTION('axis',(0.,0.,1.));
#10809=DIRECTION('refdir',(1.,0.,0.));
#10810=DIRECTION('center_axis',(0.,0.,1.));
#10811=DIRECTION('ref_axis',(1.,0.,0.));
#10812=DIRECTION('center_axis',(0.,0.,-1.));
#10813=DIRECTION('ref_axis',(1.,0.,0.));
#10814=DIRECTION('',(0.,0.,-1.));
#10815=DIRECTION('center_axis',(0.,0.,-1.));
#10816=DIRECTION('ref_axis',(1.,0.,0.));
#10817=DIRECTION('center_axis',(0.,0.,1.));
#10818=DIRECTION('ref_axis',(1.,0.,0.));
#10819=DIRECTION('center_axis',(0.,0.,1.));
#10820=DIRECTION('ref_axis',(1.,0.,0.));
#10821=DIRECTION('',(0.,0.,-1.));
#10822=DIRECTION('center_axis',(0.,0.,1.));
#10823=DIRECTION('ref_axis',(1.,0.,0.));
#10824=DIRECTION('center_axis',(0.,0.,1.));
#10825=DIRECTION('ref_axis',(1.,0.,0.));
#10826=DIRECTION('center_axis',(0.,0.,1.));
#10827=DIRECTION('ref_axis',(1.,0.,0.));
#10828=DIRECTION('axis',(0.,0.,1.));
#10829=DIRECTION('refdir',(1.,0.,0.));
#10830=DIRECTION('center_axis',(0.,0.,1.));
#10831=DIRECTION('ref_axis',(1.,0.,0.));
#10832=DIRECTION('center_axis',(0.,0.,1.));
#10833=DIRECTION('ref_axis',(1.,0.,0.));
#10834=DIRECTION('',(0.,0.,1.));
#10835=DIRECTION('center_axis',(0.,0.,-1.));
#10836=DIRECTION('ref_axis',(1.,0.,0.));
#10837=DIRECTION('center_axis',(0.,0.,1.));
#10838=DIRECTION('ref_axis',(1.,0.,0.));
#10839=DIRECTION('center_axis',(0.,0.,1.));
#10840=DIRECTION('ref_axis',(1.,0.,0.));
#10841=DIRECTION('center_axis',(0.,0.,1.));
#10842=DIRECTION('ref_axis',(1.,0.,0.));
#10843=DIRECTION('',(0.,0.,1.));
#10844=DIRECTION('center_axis',(0.,0.,-1.));
#10845=DIRECTION('ref_axis',(1.,0.,0.));
#10846=DIRECTION('center_axis',(0.,0.,1.));
#10847=DIRECTION('ref_axis',(1.,0.,0.));
#10848=DIRECTION('center_axis',(0.,0.,1.));
#10849=DIRECTION('ref_axis',(1.,0.,0.));
#10850=DIRECTION('center_axis',(0.,0.,1.));
#10851=DIRECTION('ref_axis',(1.,0.,0.));
#10852=DIRECTION('',(0.,0.,1.));
#10853=DIRECTION('center_axis',(0.,0.,-1.));
#10854=DIRECTION('ref_axis',(1.,0.,0.));
#10855=DIRECTION('center_axis',(0.,0.,1.));
#10856=DIRECTION('ref_axis',(1.,0.,0.));
#10857=DIRECTION('center_axis',(0.,0.,1.));
#10858=DIRECTION('ref_axis',(1.,0.,0.));
#10859=DIRECTION('center_axis',(0.,0.,1.));
#10860=DIRECTION('ref_axis',(1.,0.,0.));
#10861=DIRECTION('center_axis',(0.,0.,1.));
#10862=DIRECTION('ref_axis',(1.,0.,0.));
#10863=DIRECTION('',(0.,0.,1.));
#10864=DIRECTION('center_axis',(0.,0.,-1.));
#10865=DIRECTION('ref_axis',(1.,0.,0.));
#10866=DIRECTION('center_axis',(0.,0.,1.));
#10867=DIRECTION('ref_axis',(1.,0.,0.));
#10868=DIRECTION('center_axis',(0.,0.,1.));
#10869=DIRECTION('ref_axis',(1.,0.,0.));
#10870=DIRECTION('center_axis',(0.,0.,1.));
#10871=DIRECTION('ref_axis',(1.,0.,0.));
#10872=DIRECTION('center_axis',(0.,0.,1.));
#10873=DIRECTION('ref_axis',(1.,0.,0.));
#10874=DIRECTION('',(0.,0.,1.));
#10875=DIRECTION('center_axis',(0.,0.,-1.));
#10876=DIRECTION('ref_axis',(1.,0.,0.));
#10877=DIRECTION('center_axis',(0.,0.,1.));
#10878=DIRECTION('ref_axis',(1.,0.,0.));
#10879=DIRECTION('center_axis',(0.,0.,1.));
#10880=DIRECTION('ref_axis',(1.,0.,0.));
#10881=DIRECTION('center_axis',(0.,0.,1.));
#10882=DIRECTION('ref_axis',(1.,0.,0.));
#10883=DIRECTION('center_axis',(0.,0.,1.));
#10884=DIRECTION('ref_axis',(1.,0.,0.));
#10885=DIRECTION('',(0.,0.,1.));
#10886=DIRECTION('center_axis',(0.,0.,-1.));
#10887=DIRECTION('ref_axis',(1.,0.,0.));
#10888=DIRECTION('center_axis',(0.,0.,1.));
#10889=DIRECTION('ref_axis',(1.,0.,0.));
#10890=DIRECTION('center_axis',(0.,0.,1.));
#10891=DIRECTION('ref_axis',(1.,0.,0.));
#10892=DIRECTION('center_axis',(0.,0.,1.));
#10893=DIRECTION('ref_axis',(1.,0.,0.));
#10894=DIRECTION('center_axis',(0.,0.,1.));
#10895=DIRECTION('ref_axis',(1.,0.,0.));
#10896=DIRECTION('',(0.,0.,1.));
#10897=DIRECTION('center_axis',(0.,0.,1.));
#10898=DIRECTION('ref_axis',(1.,0.,0.));
#10899=DIRECTION('center_axis',(0.,0.,1.));
#10900=DIRECTION('ref_axis',(1.,0.,0.));
#10901=DIRECTION('',(0.,0.,1.));
#10902=DIRECTION('center_axis',(0.,0.,1.));
#10903=DIRECTION('ref_axis',(1.,0.,0.));
#10904=DIRECTION('center_axis',(0.,0.,1.));
#10905=DIRECTION('ref_axis',(1.,0.,0.));
#10906=DIRECTION('',(0.,0.,1.));
#10907=DIRECTION('center_axis',(0.,0.,1.));
#10908=DIRECTION('ref_axis',(1.,0.,0.));
#10909=DIRECTION('center_axis',(0.,0.,1.));
#10910=DIRECTION('ref_axis',(1.,0.,0.));
#10911=DIRECTION('',(0.,0.,1.));
#10912=DIRECTION('center_axis',(0.,1.,0.));
#10913=DIRECTION('ref_axis',(-1.,0.,0.));
#10914=DIRECTION('',(-1.,0.,0.));
#10915=DIRECTION('',(0.,0.,1.));
#10916=DIRECTION('',(-1.,0.,0.));
#10917=DIRECTION('',(0.,0.,1.));
#10918=DIRECTION('center_axis',(1.,0.,0.));
#10919=DIRECTION('ref_axis',(0.,1.,0.));
#10920=DIRECTION('',(0.,1.,0.));
#10921=DIRECTION('',(0.,1.,0.));
#10922=DIRECTION('',(0.,0.,1.));
#10923=DIRECTION('center_axis',(0.,-1.,0.));
#10924=DIRECTION('ref_axis',(1.,0.,0.));
#10925=DIRECTION('',(1.,0.,0.));
#10926=DIRECTION('',(1.,0.,0.));
#10927=DIRECTION('',(0.,0.,1.));
#10928=DIRECTION('center_axis',(-1.,0.,0.));
#10929=DIRECTION('ref_axis',(0.,-1.,0.));
#10930=DIRECTION('',(0.,-1.,0.));
#10931=DIRECTION('',(0.,-1.,0.));
#10932=DIRECTION('center_axis',(0.,0.,1.));
#10933=DIRECTION('ref_axis',(1.,0.,0.));
#10934=DIRECTION('center_axis',(0.,0.,1.));
#10935=DIRECTION('ref_axis',(1.,0.,0.));
#10936=DIRECTION('axis',(0.,0.,1.));
#10937=DIRECTION('refdir',(1.,0.,0.));
#10938=DIRECTION('center_axis',(0.,0.,1.));
#10939=DIRECTION('ref_axis',(1.,0.,0.));
#10940=DIRECTION('center_axis',(0.,0.,-1.));
#10941=DIRECTION('ref_axis',(1.,0.,0.));
#10942=DIRECTION('',(0.,0.,-1.));
#10943=DIRECTION('center_axis',(0.,0.,-1.));
#10944=DIRECTION('ref_axis',(1.,0.,0.));
#10945=DIRECTION('center_axis',(0.,0.,1.));
#10946=DIRECTION('ref_axis',(1.,0.,0.));
#10947=DIRECTION('center_axis',(0.,0.,1.));
#10948=DIRECTION('ref_axis',(1.,0.,0.));
#10949=DIRECTION('',(0.,0.,-1.));
#10950=DIRECTION('center_axis',(0.,0.,1.));
#10951=DIRECTION('ref_axis',(1.,0.,0.));
#10952=DIRECTION('center_axis',(0.,0.,1.));
#10953=DIRECTION('ref_axis',(1.,0.,0.));
#10954=DIRECTION('center_axis',(0.,0.,1.));
#10955=DIRECTION('ref_axis',(1.,0.,0.));
#10956=DIRECTION('axis',(0.,0.,1.));
#10957=DIRECTION('refdir',(1.,0.,0.));
#10958=DIRECTION('center_axis',(0.,0.,1.));
#10959=DIRECTION('ref_axis',(1.,0.,0.));
#10960=DIRECTION('center_axis',(0.,0.,-1.));
#10961=DIRECTION('ref_axis',(1.,0.,0.));
#10962=DIRECTION('',(0.,0.,-1.));
#10963=DIRECTION('center_axis',(0.,0.,-1.));
#10964=DIRECTION('ref_axis',(1.,0.,0.));
#10965=DIRECTION('center_axis',(0.,0.,1.));
#10966=DIRECTION('ref_axis',(1.,0.,0.));
#10967=DIRECTION('center_axis',(0.,0.,1.));
#10968=DIRECTION('ref_axis',(1.,0.,0.));
#10969=DIRECTION('',(0.,0.,-1.));
#10970=DIRECTION('center_axis',(0.,0.,1.));
#10971=DIRECTION('ref_axis',(1.,0.,0.));
#10972=DIRECTION('center_axis',(0.,0.,1.));
#10973=DIRECTION('ref_axis',(1.,0.,0.));
#10974=DIRECTION('center_axis',(0.,0.,1.));
#10975=DIRECTION('ref_axis',(1.,0.,0.));
#10976=DIRECTION('axis',(0.,0.,1.));
#10977=DIRECTION('refdir',(1.,0.,0.));
#10978=DIRECTION('center_axis',(0.,0.,1.));
#10979=DIRECTION('ref_axis',(1.,0.,0.));
#10980=DIRECTION('center_axis',(0.,0.,1.));
#10981=DIRECTION('ref_axis',(1.,0.,0.));
#10982=DIRECTION('',(0.,0.,1.));
#10983=DIRECTION('center_axis',(0.,0.,-1.));
#10984=DIRECTION('ref_axis',(1.,0.,0.));
#10985=DIRECTION('center_axis',(0.,0.,1.));
#10986=DIRECTION('ref_axis',(1.,0.,0.));
#10987=DIRECTION('center_axis',(0.,0.,1.));
#10988=DIRECTION('ref_axis',(1.,0.,0.));
#10989=DIRECTION('center_axis',(0.,0.,1.));
#10990=DIRECTION('ref_axis',(1.,0.,0.));
#10991=DIRECTION('',(0.,0.,1.));
#10992=DIRECTION('center_axis',(0.,0.,-1.));
#10993=DIRECTION('ref_axis',(1.,0.,0.));
#10994=DIRECTION('center_axis',(0.,0.,1.));
#10995=DIRECTION('ref_axis',(1.,0.,0.));
#10996=DIRECTION('center_axis',(0.,0.,1.));
#10997=DIRECTION('ref_axis',(1.,0.,0.));
#10998=DIRECTION('center_axis',(0.,0.,1.));
#10999=DIRECTION('ref_axis',(1.,0.,0.));
#11000=DIRECTION('',(0.,0.,1.));
#11001=DIRECTION('center_axis',(0.,0.,-1.));
#11002=DIRECTION('ref_axis',(1.,0.,0.));
#11003=DIRECTION('center_axis',(0.,0.,1.));
#11004=DIRECTION('ref_axis',(1.,0.,0.));
#11005=DIRECTION('center_axis',(0.,0.,1.));
#11006=DIRECTION('ref_axis',(1.,0.,0.));
#11007=DIRECTION('center_axis',(0.,0.,1.));
#11008=DIRECTION('ref_axis',(1.,0.,0.));
#11009=DIRECTION('',(0.,0.,1.));
#11010=DIRECTION('center_axis',(0.,0.,-1.));
#11011=DIRECTION('ref_axis',(1.,0.,0.));
#11012=DIRECTION('center_axis',(0.,0.,1.));
#11013=DIRECTION('ref_axis',(1.,0.,0.));
#11014=DIRECTION('center_axis',(0.,0.,1.));
#11015=DIRECTION('ref_axis',(1.,0.,0.));
#11016=DIRECTION('center_axis',(0.,0.,1.));
#11017=DIRECTION('ref_axis',(1.,0.,0.));
#11018=DIRECTION('',(0.,0.,1.));
#11019=DIRECTION('center_axis',(0.,0.,-1.));
#11020=DIRECTION('ref_axis',(1.,0.,0.));
#11021=DIRECTION('center_axis',(0.,0.,1.));
#11022=DIRECTION('ref_axis',(1.,0.,0.));
#11023=DIRECTION('center_axis',(0.,0.,1.));
#11024=DIRECTION('ref_axis',(1.,0.,0.));
#11025=DIRECTION('center_axis',(0.,0.,1.));
#11026=DIRECTION('ref_axis',(1.,0.,0.));
#11027=DIRECTION('center_axis',(0.,0.,1.));
#11028=DIRECTION('ref_axis',(1.,0.,0.));
#11029=DIRECTION('',(0.,0.,1.));
#11030=DIRECTION('center_axis',(0.,0.,-1.));
#11031=DIRECTION('ref_axis',(1.,0.,0.));
#11032=DIRECTION('center_axis',(0.,0.,1.));
#11033=DIRECTION('ref_axis',(1.,0.,0.));
#11034=DIRECTION('center_axis',(0.,0.,1.));
#11035=DIRECTION('ref_axis',(1.,0.,0.));
#11036=DIRECTION('center_axis',(0.,0.,1.));
#11037=DIRECTION('ref_axis',(1.,0.,0.));
#11038=DIRECTION('center_axis',(0.,0.,1.));
#11039=DIRECTION('ref_axis',(1.,0.,0.));
#11040=DIRECTION('',(0.,0.,1.));
#11041=DIRECTION('center_axis',(0.,0.,-1.));
#11042=DIRECTION('ref_axis',(1.,0.,0.));
#11043=DIRECTION('center_axis',(0.,0.,1.));
#11044=DIRECTION('ref_axis',(1.,0.,0.));
#11045=DIRECTION('center_axis',(0.,0.,1.));
#11046=DIRECTION('ref_axis',(1.,0.,0.));
#11047=DIRECTION('center_axis',(0.,0.,1.));
#11048=DIRECTION('ref_axis',(1.,0.,0.));
#11049=DIRECTION('center_axis',(0.,0.,1.));
#11050=DIRECTION('ref_axis',(1.,0.,0.));
#11051=DIRECTION('',(0.,0.,1.));
#11052=DIRECTION('center_axis',(0.,0.,-1.));
#11053=DIRECTION('ref_axis',(1.,0.,0.));
#11054=DIRECTION('center_axis',(0.,0.,1.));
#11055=DIRECTION('ref_axis',(1.,0.,0.));
#11056=DIRECTION('center_axis',(0.,0.,1.));
#11057=DIRECTION('ref_axis',(1.,0.,0.));
#11058=DIRECTION('center_axis',(0.,0.,1.));
#11059=DIRECTION('ref_axis',(1.,0.,0.));
#11060=DIRECTION('center_axis',(0.,0.,1.));
#11061=DIRECTION('ref_axis',(1.,0.,0.));
#11062=DIRECTION('',(0.,0.,1.));
#11063=DIRECTION('center_axis',(0.,0.,1.));
#11064=DIRECTION('ref_axis',(1.,0.,0.));
#11065=DIRECTION('center_axis',(0.,0.,1.));
#11066=DIRECTION('ref_axis',(1.,0.,0.));
#11067=DIRECTION('',(0.,0.,1.));
#11068=DIRECTION('center_axis',(0.,0.,1.));
#11069=DIRECTION('ref_axis',(1.,0.,0.));
#11070=DIRECTION('center_axis',(0.,0.,1.));
#11071=DIRECTION('ref_axis',(1.,0.,0.));
#11072=DIRECTION('',(0.,0.,1.));
#11073=DIRECTION('center_axis',(0.,0.,1.));
#11074=DIRECTION('ref_axis',(1.,0.,0.));
#11075=DIRECTION('center_axis',(0.,0.,1.));
#11076=DIRECTION('ref_axis',(1.,0.,0.));
#11077=DIRECTION('',(0.,0.,1.));
#11078=DIRECTION('center_axis',(0.,1.,0.));
#11079=DIRECTION('ref_axis',(-1.,0.,0.));
#11080=DIRECTION('',(-1.,0.,0.));
#11081=DIRECTION('',(0.,0.,1.));
#11082=DIRECTION('',(-1.,0.,0.));
#11083=DIRECTION('',(0.,0.,1.));
#11084=DIRECTION('center_axis',(1.,0.,0.));
#11085=DIRECTION('ref_axis',(0.,1.,0.));
#11086=DIRECTION('',(0.,1.,0.));
#11087=DIRECTION('',(0.,1.,0.));
#11088=DIRECTION('',(0.,0.,1.));
#11089=DIRECTION('center_axis',(0.,-1.,0.));
#11090=DIRECTION('ref_axis',(1.,0.,0.));
#11091=DIRECTION('',(1.,0.,0.));
#11092=DIRECTION('',(1.,0.,0.));
#11093=DIRECTION('',(0.,0.,1.));
#11094=DIRECTION('center_axis',(-1.,0.,0.));
#11095=DIRECTION('ref_axis',(0.,-1.,0.));
#11096=DIRECTION('',(0.,-1.,0.));
#11097=DIRECTION('',(0.,-1.,0.));
#11098=DIRECTION('center_axis',(0.,0.,1.));
#11099=DIRECTION('ref_axis',(1.,0.,0.));
#11100=DIRECTION('center_axis',(0.,0.,1.));
#11101=DIRECTION('ref_axis',(1.,0.,0.));
#11102=DIRECTION('axis',(0.,0.,1.));
#11103=DIRECTION('refdir',(1.,0.,0.));
#11104=DIRECTION('center_axis',(0.,1.,0.));
#11105=DIRECTION('ref_axis',(-1.,0.,0.));
#11106=DIRECTION('',(-1.,0.,0.));
#11107=DIRECTION('',(0.,0.,1.));
#11108=DIRECTION('',(-1.,0.,0.));
#11109=DIRECTION('',(0.,0.,1.));
#11110=DIRECTION('center_axis',(1.,0.,0.));
#11111=DIRECTION('ref_axis',(0.,1.,0.));
#11112=DIRECTION('',(0.,1.,0.));
#11113=DIRECTION('',(0.,1.,0.));
#11114=DIRECTION('',(0.,0.,1.));
#11115=DIRECTION('center_axis',(0.,-1.,0.));
#11116=DIRECTION('ref_axis',(1.,0.,0.));
#11117=DIRECTION('',(1.,0.,0.));
#11118=DIRECTION('',(1.,0.,0.));
#11119=DIRECTION('',(0.,0.,1.));
#11120=DIRECTION('center_axis',(-1.,0.,0.));
#11121=DIRECTION('ref_axis',(0.,-1.,0.));
#11122=DIRECTION('',(0.,-1.,0.));
#11123=DIRECTION('',(0.,-1.,0.));
#11124=DIRECTION('center_axis',(0.,0.,1.));
#11125=DIRECTION('ref_axis',(1.,0.,0.));
#11126=DIRECTION('center_axis',(0.,0.,1.));
#11127=DIRECTION('ref_axis',(1.,0.,0.));
#11128=DIRECTION('axis',(0.,0.,1.));
#11129=DIRECTION('refdir',(1.,0.,0.));
#11130=DIRECTION('center_axis',(0.,1.,0.));
#11131=DIRECTION('ref_axis',(-1.,0.,0.));
#11132=DIRECTION('',(-1.,0.,0.));
#11133=DIRECTION('',(0.,0.,1.));
#11134=DIRECTION('',(-1.,0.,0.));
#11135=DIRECTION('',(0.,0.,1.));
#11136=DIRECTION('center_axis',(1.,0.,0.));
#11137=DIRECTION('ref_axis',(0.,1.,0.));
#11138=DIRECTION('',(0.,1.,0.));
#11139=DIRECTION('',(0.,1.,0.));
#11140=DIRECTION('',(0.,0.,1.));
#11141=DIRECTION('center_axis',(0.,-1.,0.));
#11142=DIRECTION('ref_axis',(1.,0.,0.));
#11143=DIRECTION('',(1.,0.,0.));
#11144=DIRECTION('',(1.,0.,0.));
#11145=DIRECTION('',(0.,0.,1.));
#11146=DIRECTION('center_axis',(-1.,0.,0.));
#11147=DIRECTION('ref_axis',(0.,-1.,0.));
#11148=DIRECTION('',(0.,-1.,0.));
#11149=DIRECTION('',(0.,-1.,0.));
#11150=DIRECTION('center_axis',(0.,0.,1.));
#11151=DIRECTION('ref_axis',(1.,0.,0.));
#11152=DIRECTION('center_axis',(0.,0.,1.));
#11153=DIRECTION('ref_axis',(1.,0.,0.));
#11154=DIRECTION('axis',(0.,0.,1.));
#11155=DIRECTION('refdir',(1.,0.,0.));
#11156=DIRECTION('axis',(0.,0.,1.));
#11157=DIRECTION('refdir',(1.,0.,0.));
#11158=DIRECTION('center_axis',(0.,1.,0.));
#11159=DIRECTION('ref_axis',(1.,0.,0.));
#11160=DIRECTION('center_axis',(0.,1.,0.));
#11161=DIRECTION('ref_axis',(1.,0.,0.));
#11162=DIRECTION('',(0.,1.,0.));
#11163=DIRECTION('center_axis',(0.,-1.,0.));
#11164=DIRECTION('ref_axis',(1.,0.,0.));
#11165=DIRECTION('center_axis',(0.,1.,0.));
#11166=DIRECTION('ref_axis',(1.,0.,0.));
#11167=DIRECTION('center_axis',(0.,1.,0.));
#11168=DIRECTION('ref_axis',(1.,0.,0.));
#11169=DIRECTION('',(0.,1.,0.));
#11170=DIRECTION('center_axis',(0.,-1.,0.));
#11171=DIRECTION('ref_axis',(1.,0.,0.));
#11172=DIRECTION('center_axis',(6.12323399573677E-17,0.,1.));
#11173=DIRECTION('ref_axis',(1.,0.,0.));
#11174=DIRECTION('center_axis',(-1.22464679914735E-16,1.,0.));
#11175=DIRECTION('ref_axis',(-1.,-1.22464679914735E-16,0.));
#11176=DIRECTION('center_axis',(0.,1.,0.));
#11177=DIRECTION('ref_axis',(0.,0.,1.));
#11178=DIRECTION('',(1.,0.,0.));
#11179=DIRECTION('',(0.850265146687862,0.,0.526354614616295));
#11180=DIRECTION('center_axis',(0.,1.,0.));
#11181=DIRECTION('ref_axis',(1.,0.,0.));
#11182=DIRECTION('center_axis',(0.,1.,0.));
#11183=DIRECTION('ref_axis',(0.,0.,1.));
#11184=DIRECTION('',(1.,0.,0.));
#11185=DIRECTION('center_axis',(0.,1.,0.));
#11186=DIRECTION('ref_axis',(1.,0.,0.));
#11187=DIRECTION('',(0.850265146687862,0.,-0.526354614616295));
#11188=DIRECTION('center_axis',(0.,-1.,0.));
#11189=DIRECTION('ref_axis',(0.,0.,-1.));
#11190=DIRECTION('',(-1.,0.,0.));
#11191=DIRECTION('center_axis',(0.,-1.,0.));
#11192=DIRECTION('ref_axis',(1.,0.,0.));
#11193=DIRECTION('',(-0.850265146687862,0.,-0.526354614616295));
#11194=DIRECTION('center_axis',(-0.526354614616295,0.,0.850265146687862));
#11195=DIRECTION('ref_axis',(0.850265146687862,0.,0.526354614616295));
#11196=DIRECTION('',(0.,1.,0.));
#11197=DIRECTION('',(0.,-1.,0.));
#11198=DIRECTION('center_axis',(0.,-1.,0.));
#11199=DIRECTION('ref_axis',(0.,0.,-1.));
#11200=DIRECTION('',(-1.,0.,0.));
#11201=DIRECTION('',(-0.850265146687862,0.,0.526354614616295));
#11202=DIRECTION('center_axis',(0.,-1.,0.));
#11203=DIRECTION('ref_axis',(1.,0.,0.));
#11204=DIRECTION('center_axis',(0.526354614616295,0.,0.850265146687862));
#11205=DIRECTION('ref_axis',(0.850265146687862,0.,-0.526354614616295));
#11206=DIRECTION('',(0.,-1.,0.));
#11207=DIRECTION('',(0.,1.,0.));
#11208=DIRECTION('center_axis',(0.,0.,1.));
#11209=DIRECTION('ref_axis',(1.,0.,0.));
#11210=DIRECTION('',(0.,-1.,0.));
#11211=DIRECTION('',(1.,0.,0.));
#11212=DIRECTION('',(0.,1.,0.));
#11213=DIRECTION('',(-1.,0.,0.));
#11214=DIRECTION('center_axis',(0.,0.,-1.));
#11215=DIRECTION('ref_axis',(1.,0.,0.));
#11216=DIRECTION('center_axis',(0.,0.,-1.));
#11217=DIRECTION('ref_axis',(1.,0.,0.));
#11218=DIRECTION('',(0.,-1.,0.));
#11219=DIRECTION('',(-1.,0.,0.));
#11220=DIRECTION('',(0.,1.,0.));
#11221=DIRECTION('',(0.,1.,0.));
#11222=DIRECTION('',(1.,0.,0.));
#11223=DIRECTION('',(0.,-1.,0.));
#11224=DIRECTION('center_axis',(0.,1.,0.));
#11225=DIRECTION('ref_axis',(6.12323399573677E-17,0.,1.));
#11226=DIRECTION('center_axis',(0.,1.,0.));
#11227=DIRECTION('ref_axis',(1.,0.,0.));
#11228=DIRECTION('center_axis',(0.,-1.,0.));
#11229=DIRECTION('ref_axis',(1.,0.,0.));
#11230=DIRECTION('center_axis',(0.,1.,0.));
#11231=DIRECTION('ref_axis',(1.,0.,0.));
#11232=DIRECTION('center_axis',(0.,1.,0.));
#11233=DIRECTION('ref_axis',(1.,0.,0.));
#11234=DIRECTION('center_axis',(0.,1.,0.));
#11235=DIRECTION('ref_axis',(-1.,0.,0.));
#11236=DIRECTION('',(-1.,0.,0.));
#11237=DIRECTION('',(0.,0.,1.));
#11238=DIRECTION('',(-1.,0.,0.));
#11239=DIRECTION('',(0.,0.,1.));
#11240=DIRECTION('center_axis',(1.,0.,0.));
#11241=DIRECTION('ref_axis',(0.,1.,0.));
#11242=DIRECTION('',(0.,1.,0.));
#11243=DIRECTION('',(0.,0.,1.));
#11244=DIRECTION('',(0.,1.,0.));
#11245=DIRECTION('center_axis',(0.,-1.,0.));
#11246=DIRECTION('ref_axis',(1.,0.,0.));
#11247=DIRECTION('',(1.,0.,0.));
#11248=DIRECTION('',(0.,0.,1.));
#11249=DIRECTION('',(1.,0.,0.));
#11250=DIRECTION('center_axis',(-1.,0.,0.));
#11251=DIRECTION('ref_axis',(0.,-1.,0.));
#11252=DIRECTION('',(0.,-1.,0.));
#11253=DIRECTION('',(0.,-1.,0.));
#11254=DIRECTION('center_axis',(0.,0.,1.));
#11255=DIRECTION('ref_axis',(1.,0.,0.));
#11256=DIRECTION('center_axis',(0.,0.,1.));
#11257=DIRECTION('ref_axis',(1.,0.,0.));
#11258=DIRECTION('center_axis',(0.,0.,1.));
#11259=DIRECTION('ref_axis',(1.,0.,0.));
#11260=DIRECTION('',(0.,0.,1.));
#11261=DIRECTION('center_axis',(0.,0.,1.));
#11262=DIRECTION('ref_axis',(1.,0.,0.));
#11263=DIRECTION('center_axis',(0.,0.,1.));
#11264=DIRECTION('ref_axis',(1.,0.,0.));
#11265=DIRECTION('',(0.,0.,1.));
#11266=DIRECTION('center_axis',(0.,1.,0.));
#11267=DIRECTION('ref_axis',(-1.,0.,0.));
#11268=DIRECTION('',(-1.,0.,0.));
#11269=DIRECTION('',(0.,0.,1.));
#11270=DIRECTION('',(0.,0.,1.));
#11271=DIRECTION('center_axis',(1.,0.,0.));
#11272=DIRECTION('ref_axis',(0.,1.,0.));
#11273=DIRECTION('',(0.,1.,0.));
#11274=DIRECTION('',(0.,0.,1.));
#11275=DIRECTION('center_axis',(0.,-1.,0.));
#11276=DIRECTION('ref_axis',(1.,0.,0.));
#11277=DIRECTION('',(1.,0.,0.));
#11278=DIRECTION('',(0.,0.,1.));
#11279=DIRECTION('center_axis',(-1.,0.,0.));
#11280=DIRECTION('ref_axis',(0.,-1.,0.));
#11281=DIRECTION('',(0.,-1.,0.));
#11282=DIRECTION('center_axis',(0.,0.,1.));
#11283=DIRECTION('ref_axis',(1.,0.,0.));
#11284=DIRECTION('axis',(0.,0.,1.));
#11285=DIRECTION('refdir',(1.,0.,0.));
#11286=DIRECTION('center_axis',(0.,-1.,0.));
#11287=DIRECTION('ref_axis',(1.,0.,0.));
#11288=DIRECTION('center_axis',(0.,-1.,0.));
#11289=DIRECTION('ref_axis',(1.,0.,0.));
#11290=DIRECTION('',(0.,1.,0.));
#11291=DIRECTION('center_axis',(0.,-1.,0.));
#11292=DIRECTION('ref_axis',(1.,0.,0.));
#11293=DIRECTION('center_axis',(0.,1.,0.));
#11294=DIRECTION('ref_axis',(0.,0.,1.));
#11295=DIRECTION('center_axis',(0.,-1.,0.));
#11296=DIRECTION('ref_axis',(1.,0.,0.));
#11297=DIRECTION('center_axis',(6.12323399573677E-17,0.,1.));
#11298=DIRECTION('ref_axis',(1.,0.,0.));
#11299=DIRECTION('center_axis',(1.22464679914735E-16,-1.,0.));
#11300=DIRECTION('ref_axis',(-1.,-1.22464679914735E-16,0.));
#11301=DIRECTION('center_axis',(0.,-1.,0.));
#11302=DIRECTION('ref_axis',(1.,0.,0.));
#11303=DIRECTION('center_axis',(0.,-1.,0.));
#11304=DIRECTION('ref_axis',(0.,0.,-1.));
#11305=DIRECTION('center_axis',(-0.866025403784438,0.,-0.5));
#11306=DIRECTION('ref_axis',(-0.5,0.,0.866025403784438));
#11307=DIRECTION('',(-0.866025403784438,0.,-0.5));
#11308=DIRECTION('center_axis',(-0.866025403784438,0.,-0.5));
#11309=DIRECTION('ref_axis',(-0.5,0.,0.866025403784438));
#11310=DIRECTION('',(-0.866025403784438,0.,-0.5));
#11311=DIRECTION('center_axis',(0.,-1.,0.));
#11312=DIRECTION('ref_axis',(1.,0.,0.));
#11313=DIRECTION('center_axis',(0.,-1.,0.));
#11314=DIRECTION('ref_axis',(1.,0.,0.));
#11315=DIRECTION('',(0.,1.,0.));
#11316=DIRECTION('center_axis',(0.,-1.,0.));
#11317=DIRECTION('ref_axis',(1.,0.,0.));
#11318=DIRECTION('center_axis',(0.866025403784439,0.,-0.5));
#11319=DIRECTION('ref_axis',(-0.5,0.,-0.866025403784439));
#11320=DIRECTION('',(0.866025403784439,0.,-0.5));
#11321=DIRECTION('center_axis',(0.866025403784439,0.,-0.5));
#11322=DIRECTION('ref_axis',(-0.5,0.,-0.866025403784439));
#11323=DIRECTION('',(0.866025403784439,0.,-0.5));
#11324=DIRECTION('center_axis',(0.,0.,1.));
#11325=DIRECTION('ref_axis',(1.,0.,0.));
#11326=DIRECTION('',(0.,0.,1.));
#11327=DIRECTION('center_axis',(0.,0.,1.));
#11328=DIRECTION('ref_axis',(1.,0.,0.));
#11329=DIRECTION('',(0.,0.,1.));
#11330=DIRECTION('center_axis',(0.,1.,0.));
#11331=DIRECTION('ref_axis',(0.,0.,1.));
#11332=DIRECTION('center_axis',(0.,-1.,0.));
#11333=DIRECTION('ref_axis',(1.,0.,0.));
#11334=DIRECTION('center_axis',(0.,1.,0.));
#11335=DIRECTION('ref_axis',(0.,0.,1.));
#11336=DIRECTION('center_axis',(0.,-1.,0.));
#11337=DIRECTION('ref_axis',(1.,0.,0.));
#11338=DIRECTION('center_axis',(0.,-1.,0.));
#11339=DIRECTION('ref_axis',(1.,0.,0.));
#11340=DIRECTION('center_axis',(0.,-1.,0.));
#11341=DIRECTION('ref_axis',(1.,0.,0.));
#11342=DIRECTION('',(0.,1.,0.));
#11343=DIRECTION('center_axis',(0.,-1.,0.));
#11344=DIRECTION('ref_axis',(0.,0.,-1.));
#11345=DIRECTION('center_axis',(0.,-1.,0.));
#11346=DIRECTION('ref_axis',(1.,0.,0.));
#11347=DIRECTION('center_axis',(0.,-1.,0.));
#11348=DIRECTION('ref_axis',(1.,0.,0.));
#11349=DIRECTION('',(0.,1.,0.));
#11350=DIRECTION('',(0.,0.,1.));
#11351=DIRECTION('',(1.,0.,0.));
#11352=DIRECTION('',(0.,0.,1.));
#11353=DIRECTION('',(1.,0.,0.));
#11354=DIRECTION('axis',(0.,0.,1.));
#11355=DIRECTION('refdir',(1.,0.,0.));
#11356=DIRECTION('center_axis',(0.,1.,0.));
#11357=DIRECTION('ref_axis',(1.,0.,0.));
#11358=DIRECTION('center_axis',(0.,-1.,0.));
#11359=DIRECTION('ref_axis',(1.,0.,0.));
#11360=DIRECTION('',(0.,-1.,0.));
#11361=DIRECTION('center_axis',(0.,-1.,0.));
#11362=DIRECTION('ref_axis',(1.,0.,0.));
#11363=DIRECTION('center_axis',(0.,1.,0.));
#11364=DIRECTION('ref_axis',(1.,0.,0.));
#11365=DIRECTION('center_axis',(0.,1.,0.));
#11366=DIRECTION('ref_axis',(1.,0.,0.));
#11367=DIRECTION('',(0.,-1.,0.));
#11368=DIRECTION('center_axis',(0.,1.,0.));
#11369=DIRECTION('ref_axis',(1.,0.,0.));
#11370=DIRECTION('center_axis',(0.,1.,0.));
#11371=DIRECTION('ref_axis',(1.,0.,0.));
#11372=DIRECTION('center_axis',(0.,1.,0.));
#11373=DIRECTION('ref_axis',(1.,0.,0.));
#11374=DIRECTION('axis',(0.,0.,1.));
#11375=DIRECTION('refdir',(1.,0.,0.));
#11376=DIRECTION('center_axis',(0.866025403784439,0.,-0.5));
#11377=DIRECTION('ref_axis',(0.5,0.,0.866025403784439));
#11378=DIRECTION('',(-0.5,0.,-0.866025403784439));
#11379=DIRECTION('',(0.,-1.,0.));
#11380=DIRECTION('',(0.5,0.,0.866025403784439));
#11381=DIRECTION('',(0.,-1.,0.));
#11382=DIRECTION('center_axis',(1.60246890531964E-16,0.,-1.));
#11383=DIRECTION('ref_axis',(1.,0.,1.60246890531964E-16));
#11384=DIRECTION('',(-1.,0.,-1.60246890531964E-16));
#11385=DIRECTION('',(0.,-1.,0.));
#11386=DIRECTION('',(1.,0.,1.60246890531964E-16));
#11387=DIRECTION('center_axis',(-0.866025403784439,0.,-0.5));
#11388=DIRECTION('ref_axis',(0.5,0.,-0.866025403784439));
#11389=DIRECTION('',(-0.5,0.,0.866025403784439));
#11390=DIRECTION('',(0.,-1.,0.));
#11391=DIRECTION('',(0.5,0.,-0.866025403784439));
#11392=DIRECTION('center_axis',(-0.866025403784439,0.,0.5));
#11393=DIRECTION('ref_axis',(-0.5,0.,-0.866025403784439));
#11394=DIRECTION('',(0.5,0.,0.866025403784439));
#11395=DIRECTION('',(0.,-1.,0.));
#11396=DIRECTION('',(-0.5,0.,-0.866025403784439));
#11397=DIRECTION('center_axis',(-1.60246890531964E-16,0.,1.));
#11398=DIRECTION('ref_axis',(-1.,0.,-1.60246890531964E-16));
#11399=DIRECTION('',(1.,0.,1.60246890531964E-16));
#11400=DIRECTION('',(0.,-1.,0.));
#11401=DIRECTION('',(-1.,0.,-1.60246890531964E-16));
#11402=DIRECTION('center_axis',(0.866025403784439,0.,0.5));
#11403=DIRECTION('ref_axis',(-0.5,0.,0.866025403784439));
#11404=DIRECTION('',(0.5,0.,-0.866025403784439));
#11405=DIRECTION('',(-0.5,0.,0.866025403784439));
#11406=DIRECTION('center_axis',(0.,1.,0.));
#11407=DIRECTION('ref_axis',(1.,0.,0.));
#11408=DIRECTION('center_axis',(0.,-1.,0.));
#11409=DIRECTION('ref_axis',(0.,0.,-1.));
#11410=DIRECTION('center_axis',(0.,1.,0.));
#11411=DIRECTION('ref_axis',(1.,0.,0.));
#11412=DIRECTION('center_axis',(0.,1.,0.));
#11413=DIRECTION('ref_axis',(1.,0.,0.));
#11414=DIRECTION('center_axis',(0.,1.,0.));
#11415=DIRECTION('ref_axis',(0.,0.,1.));
#11416=DIRECTION('center_axis',(0.,-1.,0.));
#11417=DIRECTION('ref_axis',(1.,0.,0.));
#11418=DIRECTION('center_axis',(0.,-1.,0.));
#11419=DIRECTION('ref_axis',(1.,0.,0.));
#11420=DIRECTION('center_axis',(0.,-1.,0.));
#11421=DIRECTION('ref_axis',(1.,0.,0.));
#11422=DIRECTION('',(0.707106781186548,0.707106781186547,8.65956056235493E-17));
#11423=DIRECTION('center_axis',(0.,-1.,0.));
#11424=DIRECTION('ref_axis',(1.,0.,0.));
#11425=DIRECTION('center_axis',(0.,-1.,0.));
#11426=DIRECTION('ref_axis',(1.,0.,0.));
#11427=DIRECTION('',(0.,1.,0.));
#11428=DIRECTION('center_axis',(0.,1.,0.));
#11429=DIRECTION('ref_axis',(1.,0.,0.));
#11430=DIRECTION('center_axis',(0.,-1.,0.));
#11431=DIRECTION('ref_axis',(1.,0.,0.));
#11432=DIRECTION('',(-0.707106781186548,0.707106781186547,-8.65956056235494E-17));
#11433=DIRECTION('center_axis',(0.,-1.,0.));
#11434=DIRECTION('ref_axis',(0.,0.,-1.));
#11435=DIRECTION('center_axis',(0.,-1.,0.));
#11436=DIRECTION('ref_axis',(1.,0.,0.));
#11437=DIRECTION('center_axis',(0.,1.,0.));
#11438=DIRECTION('ref_axis',(1.,0.,0.));
#11439=DIRECTION('center_axis',(0.,1.,0.));
#11440=DIRECTION('ref_axis',(1.,0.,0.));
#11441=DIRECTION('',(-0.447213595499958,0.894427190999916,-5.47678698264203E-17));
#11442=DIRECTION('center_axis',(0.,-1.,0.));
#11443=DIRECTION('ref_axis',(1.,0.,0.));
#11444=DIRECTION('',(0.,1.,0.));
#11445=DIRECTION('axis',(0.,0.,1.));
#11446=DIRECTION('refdir',(1.,0.,0.));
#11447=DIRECTION('center_axis',(0.,0.,1.));
#11448=DIRECTION('ref_axis',(1.,0.,0.));
#11449=DIRECTION('center_axis',(0.,0.,1.));
#11450=DIRECTION('ref_axis',(1.,0.,0.));
#11451=DIRECTION('',(0.,0.,1.));
#11452=DIRECTION('center_axis',(0.,0.,-1.));
#11453=DIRECTION('ref_axis',(1.,0.,0.));
#11454=DIRECTION('center_axis',(0.,0.,1.));
#11455=DIRECTION('ref_axis',(1.,0.,0.));
#11456=DIRECTION('center_axis',(0.,0.,1.));
#11457=DIRECTION('ref_axis',(1.,0.,0.));
#11458=DIRECTION('center_axis',(0.,0.,1.));
#11459=DIRECTION('ref_axis',(1.,0.,0.));
#11460=DIRECTION('center_axis',(0.,0.,1.));
#11461=DIRECTION('ref_axis',(1.,0.,0.));
#11462=DIRECTION('',(0.,0.,1.));
#11463=DIRECTION('center_axis',(0.,0.,-1.));
#11464=DIRECTION('ref_axis',(1.,0.,0.));
#11465=DIRECTION('center_axis',(0.,0.,1.));
#11466=DIRECTION('ref_axis',(1.,0.,0.));
#11467=DIRECTION('center_axis',(0.,0.,1.));
#11468=DIRECTION('ref_axis',(1.,0.,0.));
#11469=DIRECTION('center_axis',(0.,0.,1.));
#11470=DIRECTION('ref_axis',(1.,0.,0.));
#11471=DIRECTION('center_axis',(0.,0.,1.));
#11472=DIRECTION('ref_axis',(1.,0.,0.));
#11473=DIRECTION('',(0.,0.,1.));
#11474=DIRECTION('center_axis',(0.,0.,-1.));
#11475=DIRECTION('ref_axis',(1.,0.,0.));
#11476=DIRECTION('center_axis',(0.,0.,1.));
#11477=DIRECTION('ref_axis',(1.,0.,0.));
#11478=DIRECTION('center_axis',(0.,0.,1.));
#11479=DIRECTION('ref_axis',(1.,0.,0.));
#11480=DIRECTION('center_axis',(0.,0.,1.));
#11481=DIRECTION('ref_axis',(1.,0.,0.));
#11482=DIRECTION('center_axis',(0.,0.,1.));
#11483=DIRECTION('ref_axis',(1.,0.,0.));
#11484=DIRECTION('',(0.,0.,1.));
#11485=DIRECTION('center_axis',(0.,0.,-1.));
#11486=DIRECTION('ref_axis',(1.,0.,0.));
#11487=DIRECTION('center_axis',(0.,0.,1.));
#11488=DIRECTION('ref_axis',(1.,0.,0.));
#11489=DIRECTION('center_axis',(0.,0.,1.));
#11490=DIRECTION('ref_axis',(1.,0.,0.));
#11491=DIRECTION('center_axis',(0.,0.,1.));
#11492=DIRECTION('ref_axis',(1.,0.,0.));
#11493=DIRECTION('center_axis',(0.,0.,1.));
#11494=DIRECTION('ref_axis',(1.,0.,0.));
#11495=DIRECTION('',(0.,0.,1.));
#11496=DIRECTION('center_axis',(0.,0.,1.));
#11497=DIRECTION('ref_axis',(1.,0.,0.));
#11498=DIRECTION('center_axis',(0.,0.,1.));
#11499=DIRECTION('ref_axis',(1.,0.,0.));
#11500=DIRECTION('',(0.,0.,1.));
#11501=DIRECTION('center_axis',(0.,0.,1.));
#11502=DIRECTION('ref_axis',(1.,0.,0.));
#11503=DIRECTION('center_axis',(0.,0.,1.));
#11504=DIRECTION('ref_axis',(1.,0.,0.));
#11505=DIRECTION('',(0.,0.,1.));
#11506=DIRECTION('center_axis',(0.,0.,1.));
#11507=DIRECTION('ref_axis',(1.,0.,0.));
#11508=DIRECTION('center_axis',(0.,0.,1.));
#11509=DIRECTION('ref_axis',(1.,0.,0.));
#11510=DIRECTION('',(0.,0.,1.));
#11511=DIRECTION('center_axis',(0.,-0.56333682464151,0.826227342807548));
#11512=DIRECTION('ref_axis',(0.,-0.826227342807548,-0.56333682464151));
#11513=DIRECTION('',(0.,-0.826227342807548,-0.56333682464151));
#11514=DIRECTION('',(1.,0.,0.));
#11515=DIRECTION('',(0.,-0.826227342807548,-0.56333682464151));
#11516=DIRECTION('',(1.,0.,0.));
#11517=DIRECTION('center_axis',(0.,-1.,0.));
#11518=DIRECTION('ref_axis',(0.,0.,-1.));
#11519=DIRECTION('',(0.,0.,-1.));
#11520=DIRECTION('',(0.,0.,-1.));
#11521=DIRECTION('',(1.,0.,0.));
#11522=DIRECTION('center_axis',(0.,-0.56333682464151,-0.826227342807548));
#11523=DIRECTION('ref_axis',(0.,0.826227342807548,-0.56333682464151));
#11524=DIRECTION('',(0.,0.826227342807548,-0.56333682464151));
#11525=DIRECTION('',(0.,0.826227342807548,-0.56333682464151));
#11526=DIRECTION('',(1.,0.,0.));
#11527=DIRECTION('center_axis',(0.,-1.,0.));
#11528=DIRECTION('ref_axis',(0.,0.,-1.));
#11529=DIRECTION('',(0.,0.,-1.));
#11530=DIRECTION('',(0.,0.,-1.));
#11531=DIRECTION('',(1.,0.,0.));
#11532=DIRECTION('center_axis',(0.,0.,1.));
#11533=DIRECTION('ref_axis',(0.,-1.,0.));
#11534=DIRECTION('',(0.,-1.,0.));
#11535=DIRECTION('',(0.,-1.,0.));
#11536=DIRECTION('',(1.,0.,0.));
#11537=DIRECTION('center_axis',(0.,1.,0.));
#11538=DIRECTION('ref_axis',(0.,0.,1.));
#11539=DIRECTION('',(0.,0.,1.));
#11540=DIRECTION('',(0.,0.,1.));
#11541=DIRECTION('',(1.,0.,0.));
#11542=DIRECTION('center_axis',(0.,0.56333682464151,-0.826227342807548));
#11543=DIRECTION('ref_axis',(0.,0.826227342807548,0.56333682464151));
#11544=DIRECTION('',(0.,0.826227342807548,0.56333682464151));
#11545=DIRECTION('',(0.,0.826227342807548,0.56333682464151));
#11546=DIRECTION('',(1.,0.,0.));
#11547=DIRECTION('center_axis',(0.,1.,0.));
#11548=DIRECTION('ref_axis',(0.,0.,1.));
#11549=DIRECTION('',(0.,0.,1.));
#11550=DIRECTION('',(0.,0.,1.));
#11551=DIRECTION('',(1.,0.,0.));
#11552=DIRECTION('center_axis',(0.,0.56333682464151,0.826227342807548));
#11553=DIRECTION('ref_axis',(0.,-0.826227342807548,0.56333682464151));
#11554=DIRECTION('',(0.,-0.826227342807548,0.56333682464151));
#11555=DIRECTION('',(0.,-0.826227342807548,0.56333682464151));
#11556=DIRECTION('',(1.,0.,0.));
#11557=DIRECTION('center_axis',(0.,1.,0.));
#11558=DIRECTION('ref_axis',(0.,0.,1.));
#11559=DIRECTION('',(0.,0.,1.));
#11560=DIRECTION('',(0.,0.,1.));
#11561=DIRECTION('',(1.,0.,0.));
#11562=DIRECTION('center_axis',(0.,0.,-1.));
#11563=DIRECTION('ref_axis',(0.,1.,0.));
#11564=DIRECTION('',(0.,1.,0.));
#11565=DIRECTION('',(0.,1.,0.));
#11566=DIRECTION('',(1.,0.,0.));
#11567=DIRECTION('center_axis',(0.,-1.,0.));
#11568=DIRECTION('ref_axis',(0.,0.,-1.));
#11569=DIRECTION('',(0.,0.,-1.));
#11570=DIRECTION('',(0.,0.,-1.));
#11571=DIRECTION('center_axis',(1.,0.,0.));
#11572=DIRECTION('ref_axis',(0.,0.,-1.));
#11573=DIRECTION('center_axis',(1.,0.,0.));
#11574=DIRECTION('ref_axis',(0.,0.,-1.));
#11575=DIRECTION('axis',(0.,0.,1.));
#11576=DIRECTION('refdir',(1.,0.,0.));
#11577=DIRECTION('center_axis',(0.,1.,0.));
#11578=DIRECTION('ref_axis',(0.,0.,1.));
#11579=DIRECTION('center_axis',(0.,-1.,0.));
#11580=DIRECTION('ref_axis',(1.,0.,0.));
#11581=DIRECTION('center_axis',(0.,-1.,0.));
#11582=DIRECTION('ref_axis',(1.,0.,0.));
#11583=DIRECTION('center_axis',(0.,-1.,0.));
#11584=DIRECTION('ref_axis',(1.,0.,0.));
#11585=DIRECTION('',(0.707106781186547,0.707106781186548,8.65956056235493E-17));
#11586=DIRECTION('center_axis',(0.,-1.,0.));
#11587=DIRECTION('ref_axis',(1.,0.,0.));
#11588=DIRECTION('center_axis',(0.,-1.,0.));
#11589=DIRECTION('ref_axis',(1.,0.,0.));
#11590=DIRECTION('',(0.,1.,0.));
#11591=DIRECTION('center_axis',(0.,1.,0.));
#11592=DIRECTION('ref_axis',(1.,0.,0.));
#11593=DIRECTION('center_axis',(0.,-1.,0.));
#11594=DIRECTION('ref_axis',(1.,0.,0.));
#11595=DIRECTION('',(-0.707106781186547,0.707106781186548,-8.65956056235493E-17));
#11596=DIRECTION('center_axis',(0.,-1.,0.));
#11597=DIRECTION('ref_axis',(0.,0.,-1.));
#11598=DIRECTION('center_axis',(0.,-1.,0.));
#11599=DIRECTION('ref_axis',(1.,0.,0.));
#11600=DIRECTION('center_axis',(0.,1.,0.));
#11601=DIRECTION('ref_axis',(1.,0.,0.));
#11602=DIRECTION('center_axis',(0.,1.,0.));
#11603=DIRECTION('ref_axis',(1.,0.,0.));
#11604=DIRECTION('',(-0.447213595499958,0.894427190999916,-5.47678698264203E-17));
#11605=DIRECTION('center_axis',(0.,-1.,0.));
#11606=DIRECTION('ref_axis',(1.,0.,0.));
#11607=DIRECTION('center_axis',(0.,1.,0.));
#11608=DIRECTION('ref_axis',(1.,0.,0.));
#11609=DIRECTION('',(0.,1.,0.));
#11610=DIRECTION('center_axis',(0.,1.,0.));
#11611=DIRECTION('ref_axis',(1.,0.,0.));
#11612=DIRECTION('center_axis',(0.,-1.,0.));
#11613=DIRECTION('ref_axis',(1.,0.,0.));
#11614=DIRECTION('',(-0.707106781186547,0.707106781186548,-8.65956056235493E-17));
#11615=DIRECTION('center_axis',(0.,-1.,0.));
#11616=DIRECTION('ref_axis',(0.,0.,-1.));
#11617=DIRECTION('center_axis',(0.866025403784439,0.,-0.5));
#11618=DIRECTION('ref_axis',(0.5,0.,0.866025403784439));
#11619=DIRECTION('',(-0.5,0.,-0.866025403784439));
#11620=DIRECTION('',(0.,-1.,0.));
#11621=DIRECTION('',(0.5,0.,0.866025403784439));
#11622=DIRECTION('',(0.,-1.,0.));
#11623=DIRECTION('center_axis',(1.60246890531964E-16,0.,-1.));
#11624=DIRECTION('ref_axis',(1.,0.,1.60246890531964E-16));
#11625=DIRECTION('',(-1.,0.,-1.60246890531964E-16));
#11626=DIRECTION('',(0.,-1.,0.));
#11627=DIRECTION('',(1.,0.,1.60246890531964E-16));
#11628=DIRECTION('center_axis',(-0.866025403784439,0.,-0.5));
#11629=DIRECTION('ref_axis',(0.5,0.,-0.866025403784439));
#11630=DIRECTION('',(-0.5,0.,0.866025403784439));
#11631=DIRECTION('',(0.,-1.,0.));
#11632=DIRECTION('',(0.5,0.,-0.866025403784439));
#11633=DIRECTION('center_axis',(-0.866025403784439,0.,0.5));
#11634=DIRECTION('ref_axis',(-0.5,0.,-0.866025403784439));
#11635=DIRECTION('',(0.5,0.,0.866025403784439));
#11636=DIRECTION('',(0.,-1.,0.));
#11637=DIRECTION('',(-0.5,0.,-0.866025403784439));
#11638=DIRECTION('center_axis',(-1.60246890531964E-16,0.,1.));
#11639=DIRECTION('ref_axis',(-1.,0.,-1.60246890531964E-16));
#11640=DIRECTION('',(1.,0.,1.60246890531964E-16));
#11641=DIRECTION('',(0.,-1.,0.));
#11642=DIRECTION('',(-1.,0.,-1.60246890531964E-16));
#11643=DIRECTION('center_axis',(0.866025403784439,0.,0.5));
#11644=DIRECTION('ref_axis',(-0.5,0.,0.866025403784439));
#11645=DIRECTION('',(0.5,0.,-0.866025403784439));
#11646=DIRECTION('',(-0.5,0.,0.866025403784439));
#11647=DIRECTION('center_axis',(0.,1.,0.));
#11648=DIRECTION('ref_axis',(1.,0.,0.));
#11649=DIRECTION('center_axis',(0.,-1.,0.));
#11650=DIRECTION('ref_axis',(0.,0.,-1.));
#11651=DIRECTION('axis',(0.,0.,1.));
#11652=DIRECTION('refdir',(1.,0.,0.));
#11653=DIRECTION('axis',(0.,0.,1.));
#11654=DIRECTION('refdir',(1.,0.,0.));
#11655=DIRECTION('center_axis',(-1.,0.,0.));
#11656=DIRECTION('ref_axis',(0.,0.,1.));
#11657=DIRECTION('',(0.,-1.,0.));
#11658=DIRECTION('',(0.,0.,-1.));
#11659=DIRECTION('',(0.,1.,0.));
#11660=DIRECTION('',(0.,0.,-1.));
#11661=DIRECTION('center_axis',(0.,1.,0.));
#11662=DIRECTION('ref_axis',(1.,0.,0.));
#11663=DIRECTION('center_axis',(0.,-1.,0.));
#11664=DIRECTION('ref_axis',(1.,0.,0.));
#11665=DIRECTION('',(-1.,0.,0.));
#11666=DIRECTION('',(0.,0.,1.));
#11667=DIRECTION('center_axis',(1.,0.,0.));
#11668=DIRECTION('ref_axis',(0.,0.,-1.));
#11669=DIRECTION('',(0.,1.,0.));
#11670=DIRECTION('',(0.,1.,0.));
#11671=DIRECTION('',(0.,0.,1.));
#11672=DIRECTION('center_axis',(0.,0.,1.));
#11673=DIRECTION('ref_axis',(1.,0.,0.));
#11674=DIRECTION('',(-1.,0.,0.));
#11675=DIRECTION('center_axis',(0.,1.,0.));
#11676=DIRECTION('ref_axis',(1.,0.,0.));
#11677=DIRECTION('center_axis',(0.,1.,0.));
#11678=DIRECTION('ref_axis',(1.,0.,0.));
#11679=DIRECTION('',(0.,-1.,0.));
#11680=DIRECTION('center_axis',(0.,1.,0.));
#11681=DIRECTION('ref_axis',(1.,0.,0.));
#11682=DIRECTION('center_axis',(0.,1.,0.));
#11683=DIRECTION('ref_axis',(1.,0.,0.));
#11684=DIRECTION('center_axis',(0.,1.,0.));
#11685=DIRECTION('ref_axis',(1.,0.,0.));
#11686=DIRECTION('center_axis',(0.,1.,0.));
#11687=DIRECTION('ref_axis',(1.,0.,0.));
#11688=DIRECTION('axis',(0.,0.,1.));
#11689=DIRECTION('refdir',(1.,0.,0.));
#11690=DIRECTION('center_axis',(0.,0.,1.));
#11691=DIRECTION('ref_axis',(1.,0.,0.));
#11692=DIRECTION('',(0.,1.,0.));
#11693=DIRECTION('center_axis',(0.,0.,1.));
#11694=DIRECTION('ref_axis',(1.,0.,0.));
#11695=DIRECTION('center_axis',(0.,0.,1.));
#11696=DIRECTION('ref_axis',(1.,0.,0.));
#11697=DIRECTION('center_axis',(0.,0.,1.));
#11698=DIRECTION('ref_axis',(1.,0.,0.));
#11699=DIRECTION('',(0.,0.,1.));
#11700=DIRECTION('center_axis',(0.,0.,1.));
#11701=DIRECTION('ref_axis',(1.,0.,0.));
#11702=DIRECTION('center_axis',(0.,0.,1.));
#11703=DIRECTION('ref_axis',(1.,0.,0.));
#11704=DIRECTION('',(0.,-1.,0.));
#11705=DIRECTION('center_axis',(0.,1.,0.));
#11706=DIRECTION('ref_axis',(1.,0.,0.));
#11707=DIRECTION('center_axis',(0.,-1.,0.));
#11708=DIRECTION('ref_axis',(1.,0.,0.));
#11709=DIRECTION('',(0.,-1.,0.));
#11710=DIRECTION('center_axis',(0.,-1.,0.));
#11711=DIRECTION('ref_axis',(1.,0.,0.));
#11712=DIRECTION('center_axis',(0.,1.,0.));
#11713=DIRECTION('ref_axis',(1.,0.,0.));
#11714=DIRECTION('center_axis',(0.,1.,0.));
#11715=DIRECTION('ref_axis',(1.,0.,0.));
#11716=DIRECTION('',(0.,-1.,0.));
#11717=DIRECTION('center_axis',(0.,1.,0.));
#11718=DIRECTION('ref_axis',(1.,0.,0.));
#11719=DIRECTION('center_axis',(0.,1.,0.));
#11720=DIRECTION('ref_axis',(1.,0.,0.));
#11721=DIRECTION('center_axis',(0.,1.,0.));
#11722=DIRECTION('ref_axis',(1.,0.,0.));
#11723=DIRECTION('axis',(0.,0.,1.));
#11724=DIRECTION('refdir',(1.,0.,0.));
#11725=DIRECTION('center_axis',(0.,0.,1.));
#11726=DIRECTION('ref_axis',(1.,0.,0.));
#11727=DIRECTION('',(0.,1.,0.));
#11728=DIRECTION('center_axis',(0.,0.,1.));
#11729=DIRECTION('ref_axis',(1.,0.,0.));
#11730=DIRECTION('center_axis',(0.,0.,1.));
#11731=DIRECTION('ref_axis',(1.,0.,0.));
#11732=DIRECTION('center_axis',(0.,0.,1.));
#11733=DIRECTION('ref_axis',(1.,0.,0.));
#11734=DIRECTION('',(0.,0.,1.));
#11735=DIRECTION('center_axis',(0.,0.,1.));
#11736=DIRECTION('ref_axis',(1.,0.,0.));
#11737=DIRECTION('center_axis',(0.,0.,1.));
#11738=DIRECTION('ref_axis',(1.,0.,0.));
#11739=DIRECTION('',(0.,-1.,0.));
#11740=DIRECTION('center_axis',(0.,1.,0.));
#11741=DIRECTION('ref_axis',(1.,0.,0.));
#11742=DIRECTION('center_axis',(0.,-1.,0.));
#11743=DIRECTION('ref_axis',(1.,0.,0.));
#11744=DIRECTION('',(0.,-1.,0.));
#11745=DIRECTION('center_axis',(0.,-1.,0.));
#11746=DIRECTION('ref_axis',(1.,0.,0.));
#11747=DIRECTION('center_axis',(0.,1.,0.));
#11748=DIRECTION('ref_axis',(1.,0.,0.));
#11749=DIRECTION('center_axis',(0.,1.,0.));
#11750=DIRECTION('ref_axis',(1.,0.,0.));
#11751=DIRECTION('',(0.,-1.,0.));
#11752=DIRECTION('center_axis',(0.,1.,0.));
#11753=DIRECTION('ref_axis',(1.,0.,0.));
#11754=DIRECTION('center_axis',(0.,1.,0.));
#11755=DIRECTION('ref_axis',(1.,0.,0.));
#11756=DIRECTION('center_axis',(0.,1.,0.));
#11757=DIRECTION('ref_axis',(1.,0.,0.));
#11758=DIRECTION('axis',(0.,0.,1.));
#11759=DIRECTION('refdir',(1.,0.,0.));
#11760=DIRECTION('center_axis',(0.,1.,0.));
#11761=DIRECTION('ref_axis',(1.,0.,0.));
#11762=DIRECTION('center_axis',(0.,-1.,0.));
#11763=DIRECTION('ref_axis',(1.,0.,0.));
#11764=DIRECTION('',(0.,-1.,0.));
#11765=DIRECTION('center_axis',(0.,-1.,0.));
#11766=DIRECTION('ref_axis',(1.,0.,0.));
#11767=DIRECTION('center_axis',(0.,1.,0.));
#11768=DIRECTION('ref_axis',(1.,0.,0.));
#11769=DIRECTION('center_axis',(0.,1.,0.));
#11770=DIRECTION('ref_axis',(1.,0.,0.));
#11771=DIRECTION('',(0.,-1.,0.));
#11772=DIRECTION('center_axis',(0.,1.,0.));
#11773=DIRECTION('ref_axis',(1.,0.,0.));
#11774=DIRECTION('center_axis',(0.,1.,0.));
#11775=DIRECTION('ref_axis',(1.,0.,0.));
#11776=DIRECTION('center_axis',(0.,1.,0.));
#11777=DIRECTION('ref_axis',(1.,0.,0.));
#11778=DIRECTION('axis',(0.,0.,1.));
#11779=DIRECTION('refdir',(1.,0.,0.));
#11780=DIRECTION('center_axis',(0.,1.,0.));
#11781=DIRECTION('ref_axis',(1.,0.,0.));
#11782=DIRECTION('center_axis',(0.,1.,0.));
#11783=DIRECTION('ref_axis',(1.,0.,0.));
#11784=DIRECTION('center_axis',(0.,1.,0.));
#11785=DIRECTION('ref_axis',(1.,0.,0.));
#11786=DIRECTION('center_axis',(0.,1.,0.));
#11787=DIRECTION('ref_axis',(1.,0.,0.));
#11788=DIRECTION('',(0.,-1.,0.));
#11789=DIRECTION('center_axis',(0.,1.,0.));
#11790=DIRECTION('ref_axis',(1.,0.,0.));
#11791=DIRECTION('',(0.,1.,0.));
#11792=DIRECTION('center_axis',(0.,-1.,0.));
#11793=DIRECTION('ref_axis',(1.,0.,0.));
#11794=DIRECTION('center_axis',(0.,1.,0.));
#11795=DIRECTION('ref_axis',(1.,0.,0.));
#11796=DIRECTION('',(0.,1.,0.));
#11797=DIRECTION('center_axis',(0.,1.,0.));
#11798=DIRECTION('ref_axis',(6.12323399573677E-17,0.,1.));
#11799=DIRECTION('center_axis',(0.,1.,0.));
#11800=DIRECTION('ref_axis',(1.,0.,0.));
#11801=DIRECTION('',(0.,-1.,0.));
#11802=DIRECTION('center_axis',(0.,-1.,0.));
#11803=DIRECTION('ref_axis',(1.,0.,0.));
#11804=DIRECTION('',(0.,1.,0.));
#11805=DIRECTION('',(0.,-1.,0.));
#11806=DIRECTION('center_axis',(0.,-1.,0.));
#11807=DIRECTION('ref_axis',(1.,0.,0.));
#11808=DIRECTION('',(0.,1.,0.));
#11809=DIRECTION('center_axis',(0.,1.,0.));
#11810=DIRECTION('ref_axis',(1.,0.,0.));
#11811=DIRECTION('center_axis',(0.,1.,0.));
#11812=DIRECTION('ref_axis',(1.,0.,0.));
#11813=DIRECTION('',(0.,0.,1.));
#11814=DIRECTION('',(-1.,0.,0.));
#11815=DIRECTION('',(0.,0.,-1.));
#11816=DIRECTION('center_axis',(0.,1.,0.));
#11817=DIRECTION('ref_axis',(1.,0.,0.));
#11818=DIRECTION('center_axis',(0.,1.,0.));
#11819=DIRECTION('ref_axis',(1.,0.,0.));
#11820=DIRECTION('center_axis',(0.,0.,-1.));
#11821=DIRECTION('ref_axis',(-1.,0.,0.));
#11822=DIRECTION('',(0.,1.,0.));
#11823=DIRECTION('',(-1.,0.,0.));
#11824=DIRECTION('',(0.,1.,0.));
#11825=DIRECTION('center_axis',(-1.,0.,0.));
#11826=DIRECTION('ref_axis',(0.,0.,1.));
#11827=DIRECTION('',(0.,0.,1.));
#11828=DIRECTION('center_axis',(0.,0.,1.));
#11829=DIRECTION('ref_axis',(1.,0.,0.));
#11830=DIRECTION('center_axis',(0.,0.,1.));
#11831=DIRECTION('ref_axis',(1.,0.,0.));
#11832=DIRECTION('center_axis',(0.,0.,1.));
#11833=DIRECTION('ref_axis',(6.12323399573677E-17,1.,0.));
#11834=DIRECTION('center_axis',(0.,0.,1.));
#11835=DIRECTION('ref_axis',(1.,0.,0.));
#11836=DIRECTION('',(0.,0.,-1.));
#11837=DIRECTION('',(0.,0.,1.));
#11838=DIRECTION('center_axis',(0.,0.,1.));
#11839=DIRECTION('ref_axis',(1.,0.,0.));
#11840=DIRECTION('center_axis',(1.,0.,0.));
#11841=DIRECTION('ref_axis',(0.,0.,-1.));
#11842=DIRECTION('',(0.,0.,-1.));
#11843=DIRECTION('center_axis',(0.,1.,0.));
#11844=DIRECTION('ref_axis',(1.,0.,0.));
#11845=DIRECTION('center_axis',(0.,1.,0.));
#11846=DIRECTION('ref_axis',(1.,0.,0.));
#11847=DIRECTION('center_axis',(0.,-1.,0.));
#11848=DIRECTION('ref_axis',(1.,0.,0.));
#11849=DIRECTION('center_axis',(0.,1.,0.));
#11850=DIRECTION('ref_axis',(1.,0.,0.));
#11851=DIRECTION('',(0.,-1.,0.));
#11852=DIRECTION('center_axis',(0.,1.,0.));
#11853=DIRECTION('ref_axis',(1.,0.,0.));
#11854=DIRECTION('',(0.,-1.,0.));
#11855=DIRECTION('center_axis',(0.,1.,0.));
#11856=DIRECTION('ref_axis',(1.,0.,0.));
#11857=DIRECTION('center_axis',(0.,1.,0.));
#11858=DIRECTION('ref_axis',(1.,0.,0.));
#11859=DIRECTION('center_axis',(0.,1.,0.));
#11860=DIRECTION('ref_axis',(1.,0.,0.));
#11861=DIRECTION('axis',(0.,0.,1.));
#11862=DIRECTION('refdir',(1.,0.,0.));
#11863=DIRECTION('center_axis',(0.,1.,0.));
#11864=DIRECTION('ref_axis',(1.,0.,0.));
#11865=DIRECTION('center_axis',(0.,1.,0.));
#11866=DIRECTION('ref_axis',(1.,0.,0.));
#11867=DIRECTION('',(0.,1.,0.));
#11868=DIRECTION('center_axis',(0.,-1.,0.));
#11869=DIRECTION('ref_axis',(1.,0.,0.));
#11870=DIRECTION('center_axis',(0.,1.,0.));
#11871=DIRECTION('ref_axis',(1.,0.,0.));
#11872=DIRECTION('center_axis',(0.,1.,0.));
#11873=DIRECTION('ref_axis',(1.,0.,0.));
#11874=DIRECTION('center_axis',(0.,1.,0.));
#11875=DIRECTION('ref_axis',(1.,0.,0.));
#11876=DIRECTION('center_axis',(0.,1.,0.));
#11877=DIRECTION('ref_axis',(1.,0.,0.));
#11878=DIRECTION('center_axis',(0.,1.,0.));
#11879=DIRECTION('ref_axis',(1.,0.,0.));
#11880=DIRECTION('center_axis',(0.,1.,0.));
#11881=DIRECTION('ref_axis',(1.,0.,0.));
#11882=DIRECTION('',(0.,-1.,0.));
#11883=DIRECTION('center_axis',(0.,1.,0.));
#11884=DIRECTION('ref_axis',(1.,0.,0.));
#11885=DIRECTION('center_axis',(0.,1.,0.));
#11886=DIRECTION('ref_axis',(1.,0.,0.));
#11887=DIRECTION('',(0.,-1.,0.));
#11888=DIRECTION('center_axis',(0.,1.,0.));
#11889=DIRECTION('ref_axis',(1.,0.,0.));
#11890=DIRECTION('center_axis',(0.,1.,0.));
#11891=DIRECTION('ref_axis',(1.,0.,0.));
#11892=DIRECTION('axis',(0.,0.,1.));
#11893=DIRECTION('refdir',(1.,0.,0.));
#11894=DIRECTION('center_axis',(0.,1.,0.));
#11895=DIRECTION('ref_axis',(1.,0.,0.));
#11896=DIRECTION('center_axis',(0.,-1.,0.));
#11897=DIRECTION('ref_axis',(1.,0.,0.));
#11898=DIRECTION('',(0.,-1.,0.));
#11899=DIRECTION('center_axis',(0.,-1.,0.));
#11900=DIRECTION('ref_axis',(1.,0.,0.));
#11901=DIRECTION('center_axis',(0.,1.,0.));
#11902=DIRECTION('ref_axis',(1.,0.,0.));
#11903=DIRECTION('center_axis',(0.,1.,0.));
#11904=DIRECTION('ref_axis',(1.,0.,0.));
#11905=DIRECTION('',(0.,-1.,0.));
#11906=DIRECTION('center_axis',(0.,1.,0.));
#11907=DIRECTION('ref_axis',(1.,0.,0.));
#11908=DIRECTION('center_axis',(0.,1.,0.));
#11909=DIRECTION('ref_axis',(1.,0.,0.));
#11910=DIRECTION('center_axis',(0.,1.,0.));
#11911=DIRECTION('ref_axis',(1.,0.,0.));
#11912=DIRECTION('axis',(0.,0.,1.));
#11913=DIRECTION('refdir',(1.,0.,0.));
#11914=DIRECTION('center_axis',(0.,1.,0.));
#11915=DIRECTION('ref_axis',(1.,0.,0.));
#11916=DIRECTION('center_axis',(0.,-1.,0.));
#11917=DIRECTION('ref_axis',(1.,0.,0.));
#11918=DIRECTION('',(0.,-1.,0.));
#11919=DIRECTION('center_axis',(0.,-1.,0.));
#11920=DIRECTION('ref_axis',(1.,0.,0.));
#11921=DIRECTION('center_axis',(0.,1.,0.));
#11922=DIRECTION('ref_axis',(1.,0.,0.));
#11923=DIRECTION('center_axis',(0.,1.,0.));
#11924=DIRECTION('ref_axis',(1.,0.,0.));
#11925=DIRECTION('',(0.,-1.,0.));
#11926=DIRECTION('center_axis',(0.,1.,0.));
#11927=DIRECTION('ref_axis',(1.,0.,0.));
#11928=DIRECTION('center_axis',(0.,1.,0.));
#11929=DIRECTION('ref_axis',(1.,0.,0.));
#11930=DIRECTION('center_axis',(0.,1.,0.));
#11931=DIRECTION('ref_axis',(1.,0.,0.));
#11932=DIRECTION('axis',(0.,0.,1.));
#11933=DIRECTION('refdir',(1.,0.,0.));
#11934=DIRECTION('center_axis',(0.,1.,0.));
#11935=DIRECTION('ref_axis',(1.,0.,0.));
#11936=DIRECTION('center_axis',(0.,-1.,0.));
#11937=DIRECTION('ref_axis',(1.,0.,0.));
#11938=DIRECTION('',(0.,-1.,0.));
#11939=DIRECTION('center_axis',(0.,-1.,0.));
#11940=DIRECTION('ref_axis',(1.,0.,0.));
#11941=DIRECTION('center_axis',(0.,1.,0.));
#11942=DIRECTION('ref_axis',(1.,0.,0.));
#11943=DIRECTION('center_axis',(0.,1.,0.));
#11944=DIRECTION('ref_axis',(1.,0.,0.));
#11945=DIRECTION('',(0.,-1.,0.));
#11946=DIRECTION('center_axis',(0.,1.,0.));
#11947=DIRECTION('ref_axis',(1.,0.,0.));
#11948=DIRECTION('center_axis',(0.,1.,0.));
#11949=DIRECTION('ref_axis',(1.,0.,0.));
#11950=DIRECTION('center_axis',(0.,1.,0.));
#11951=DIRECTION('ref_axis',(1.,0.,0.));
#11952=DIRECTION('axis',(0.,0.,1.));
#11953=DIRECTION('refdir',(1.,0.,0.));
#11954=DIRECTION('center_axis',(1.,0.,0.));
#11955=DIRECTION('ref_axis',(0.,0.,-1.));
#11956=DIRECTION('',(0.,-0.707106781186547,-0.707106781186548));
#11957=DIRECTION('',(0.,-1.,0.));
#11958=DIRECTION('',(0.,-0.707106781186547,0.707106781186548));
#11959=DIRECTION('',(0.,0.,1.));
#11960=DIRECTION('',(0.,0.707106781186547,0.707106781186548));
#11961=DIRECTION('',(0.,1.,0.));
#11962=DIRECTION('',(0.,0.707106781186547,-0.707106781186548));
#11963=DIRECTION('',(0.,0.,-1.));
#11964=DIRECTION('center_axis',(0.,0.707106781186548,-0.707106781186547));
#11965=DIRECTION('ref_axis',(-1.,0.,0.));
#11966=DIRECTION('',(1.,0.,0.));
#11967=DIRECTION('',(0.,-0.707106781186547,-0.707106781186548));
#11968=DIRECTION('',(-1.,0.,0.));
#11969=DIRECTION('center_axis',(0.,1.,0.));
#11970=DIRECTION('ref_axis',(-1.,0.,0.));
#11971=DIRECTION('',(-1.,0.,0.));
#11972=DIRECTION('',(0.,0.,-1.));
#11973=DIRECTION('center_axis',(0.,0.707106781186548,0.707106781186547));
#11974=DIRECTION('ref_axis',(1.,0.,0.));
#11975=DIRECTION('',(1.,0.,0.));
#11976=DIRECTION('',(0.,0.707106781186547,-0.707106781186548));
#11977=DIRECTION('center_axis',(0.,0.,1.));
#11978=DIRECTION('ref_axis',(1.,0.,0.));
#11979=DIRECTION('',(-1.,0.,0.));
#11980=DIRECTION('',(0.,1.,0.));
#11981=DIRECTION('center_axis',(1.,0.,0.));
#11982=DIRECTION('ref_axis',(0.,0.,-1.));
#11983=DIRECTION('',(0.,-0.707106781186547,0.707106781186548));
#11984=DIRECTION('',(0.,-1.,0.));
#11985=DIRECTION('',(0.,0.707106781186547,0.707106781186548));
#11986=DIRECTION('',(0.,0.,1.));
#11987=DIRECTION('center_axis',(0.,0.,1.));
#11988=DIRECTION('ref_axis',(1.,0.,0.));
#11989=DIRECTION('',(1.,0.,0.));
#11990=DIRECTION('center_axis',(0.,-0.707106781186548,0.707106781186547));
#11991=DIRECTION('ref_axis',(1.,0.,0.));
#11992=DIRECTION('',(1.,0.,0.));
#11993=DIRECTION('center_axis',(0.,-0.707106781186548,-0.707106781186547));
#11994=DIRECTION('ref_axis',(-1.,0.,0.));
#11995=DIRECTION('',(-1.,0.,0.));
#11996=DIRECTION('center_axis',(0.,-1.,0.));
#11997=DIRECTION('ref_axis',(1.,0.,0.));
#11998=DIRECTION('axis',(0.,0.,1.));
#11999=DIRECTION('refdir',(1.,0.,0.));
#12000=DIRECTION('center_axis',(0.866025403784439,0.,-0.5));
#12001=DIRECTION('ref_axis',(0.5,0.,0.866025403784439));
#12002=DIRECTION('',(0.5,0.,0.866025403784439));
#12003=DIRECTION('',(0.,-1.,0.));
#12004=DIRECTION('',(0.5,0.,0.866025403784439));
#12005=DIRECTION('',(0.,-1.,0.));
#12006=DIRECTION('center_axis',(1.92296268638356E-16,0.,-1.));
#12007=DIRECTION('ref_axis',(1.,0.,1.92296268638356E-16));
#12008=DIRECTION('',(1.,0.,1.92296268638356E-16));
#12009=DIRECTION('',(0.,-1.,0.));
#12010=DIRECTION('',(1.,0.,1.92296268638356E-16));
#12011=DIRECTION('center_axis',(-0.866025403784439,0.,-0.5));
#12012=DIRECTION('ref_axis',(0.5,0.,-0.866025403784439));
#12013=DIRECTION('',(0.5,0.,-0.866025403784439));
#12014=DIRECTION('',(0.,-1.,0.));
#12015=DIRECTION('',(0.5,0.,-0.866025403784438));
#12016=DIRECTION('center_axis',(-0.866025403784439,0.,0.5));
#12017=DIRECTION('ref_axis',(-0.5,0.,-0.866025403784439));
#12018=DIRECTION('',(-0.5,0.,-0.866025403784439));
#12019=DIRECTION('',(0.,-1.,0.));
#12020=DIRECTION('',(-0.5,0.,-0.866025403784439));
#12021=DIRECTION('center_axis',(-1.92296268638356E-16,0.,1.));
#12022=DIRECTION('ref_axis',(-1.,0.,-1.92296268638356E-16));
#12023=DIRECTION('',(-1.,0.,-1.92296268638356E-16));
#12024=DIRECTION('',(0.,-1.,0.));
#12025=DIRECTION('',(-1.,0.,-1.92296268638356E-16));
#12026=DIRECTION('center_axis',(0.866025403784439,0.,0.5));
#12027=DIRECTION('ref_axis',(-0.5,0.,0.866025403784439));
#12028=DIRECTION('',(-0.5,0.,0.866025403784439));
#12029=DIRECTION('',(-0.5,0.,0.866025403784439));
#12030=DIRECTION('center_axis',(0.,-1.,0.));
#12031=DIRECTION('ref_axis',(0.,0.,-1.));
#12032=DIRECTION('center_axis',(0.,1.,0.));
#12033=DIRECTION('ref_axis',(0.,0.,1.));
#12034=DIRECTION('center_axis',(0.,-1.,0.));
#12035=DIRECTION('ref_axis',(1.,0.,0.));
#12036=DIRECTION('center_axis',(0.,-1.,0.));
#12037=DIRECTION('ref_axis',(1.,0.,0.));
#12038=DIRECTION('center_axis',(0.,-1.,0.));
#12039=DIRECTION('ref_axis',(1.,0.,0.));
#12040=DIRECTION('',(0.707106781186547,0.707106781186548,8.65956056235493E-17));
#12041=DIRECTION('center_axis',(0.,-1.,0.));
#12042=DIRECTION('ref_axis',(1.,0.,0.));
#12043=DIRECTION('center_axis',(0.,1.,0.));
#12044=DIRECTION('ref_axis',(1.,0.,0.));
#12045=DIRECTION('',(0.,1.,0.));
#12046=DIRECTION('center_axis',(0.,1.,0.));
#12047=DIRECTION('ref_axis',(1.,0.,0.));
#12048=DIRECTION('center_axis',(0.,-1.,0.));
#12049=DIRECTION('ref_axis',(1.,0.,0.));
#12050=DIRECTION('',(-0.707106781186547,0.707106781186548,-8.65956056235493E-17));
#12051=DIRECTION('center_axis',(0.,-1.,0.));
#12052=DIRECTION('ref_axis',(0.,0.,-1.));
#12053=DIRECTION('axis',(0.,0.,1.));
#12054=DIRECTION('refdir',(1.,0.,0.));
#12055=DIRECTION('axis',(0.,0.,1.));
#12056=DIRECTION('refdir',(1.,0.,0.));
#12057=DIRECTION('center_axis',(0.,1.,0.));
#12058=DIRECTION('ref_axis',(1.,0.,0.));
#12059=DIRECTION('center_axis',(0.,1.,0.));
#12060=DIRECTION('ref_axis',(1.,0.,0.));
#12061=DIRECTION('',(0.,1.,0.));
#12062=DIRECTION('center_axis',(0.,-1.,0.));
#12063=DIRECTION('ref_axis',(1.,0.,0.));
#12064=DIRECTION('center_axis',(0.,1.,0.));
#12065=DIRECTION('ref_axis',(1.,0.,0.));
#12066=DIRECTION('center_axis',(0.,1.,0.));
#12067=DIRECTION('ref_axis',(1.,0.,0.));
#12068=DIRECTION('',(0.,1.,0.));
#12069=DIRECTION('center_axis',(0.,-1.,0.));
#12070=DIRECTION('ref_axis',(1.,0.,0.));
#12071=DIRECTION('center_axis',(0.,1.,0.));
#12072=DIRECTION('ref_axis',(1.,0.,0.));
#12073=DIRECTION('',(0.,1.,0.));
#12074=DIRECTION('center_axis',(0.,1.,0.));
#12075=DIRECTION('ref_axis',(1.,0.,0.));
#12076=DIRECTION('',(0.,-1.,0.));
#12077=DIRECTION('center_axis',(0.,1.,0.));
#12078=DIRECTION('ref_axis',(1.,0.,0.));
#12079=DIRECTION('center_axis',(0.,1.,0.));
#12080=DIRECTION('ref_axis',(0.,0.,1.));
#12081=DIRECTION('',(-1.,0.,0.));
#12082=DIRECTION('center_axis',(0.,1.,0.));
#12083=DIRECTION('ref_axis',(1.,0.,0.));
#12084=DIRECTION('',(1.,0.,0.));
#12085=DIRECTION('center_axis',(0.,0.,-1.));
#12086=DIRECTION('ref_axis',(-1.,0.,0.));
#12087=DIRECTION('',(1.,0.,0.));
#12088=DIRECTION('',(0.,1.,0.));
#12089=DIRECTION('center_axis',(0.,1.,0.));
#12090=DIRECTION('ref_axis',(-1.,0.,1.22464679914735E-16));
#12091=DIRECTION('',(0.,-1.,0.));
#12092=DIRECTION('center_axis',(0.,1.,0.));
#12093=DIRECTION('ref_axis',(1.,0.,0.));
#12094=DIRECTION('center_axis',(0.,0.,1.));
#12095=DIRECTION('ref_axis',(1.,0.,0.));
#12096=DIRECTION('',(-1.,0.,0.));
#12097=DIRECTION('center_axis',(0.,1.,0.));
#12098=DIRECTION('ref_axis',(1.,0.,0.));
#12099=DIRECTION('axis',(0.,0.,1.));
#12100=DIRECTION('refdir',(1.,0.,0.));
#12101=DIRECTION('center_axis',(0.,1.,0.));
#12102=DIRECTION('ref_axis',(1.,0.,0.));
#12103=DIRECTION('center_axis',(0.,-1.,0.));
#12104=DIRECTION('ref_axis',(1.,0.,0.));
#12105=DIRECTION('',(0.,-1.,0.));
#12106=DIRECTION('center_axis',(0.,-1.,0.));
#12107=DIRECTION('ref_axis',(1.,0.,0.));
#12108=DIRECTION('center_axis',(0.,1.,0.));
#12109=DIRECTION('ref_axis',(1.,0.,0.));
#12110=DIRECTION('center_axis',(0.,1.,0.));
#12111=DIRECTION('ref_axis',(1.,0.,0.));
#12112=DIRECTION('',(0.,-1.,0.));
#12113=DIRECTION('center_axis',(0.,1.,0.));
#12114=DIRECTION('ref_axis',(1.,0.,0.));
#12115=DIRECTION('center_axis',(0.,1.,0.));
#12116=DIRECTION('ref_axis',(1.,0.,0.));
#12117=DIRECTION('center_axis',(0.,1.,0.));
#12118=DIRECTION('ref_axis',(1.,0.,0.));
#12119=DIRECTION('axis',(0.,0.,1.));
#12120=DIRECTION('refdir',(1.,0.,0.));
#12121=DIRECTION('center_axis',(0.,1.,0.));
#12122=DIRECTION('ref_axis',(1.,0.,0.));
#12123=DIRECTION('center_axis',(0.,-1.,0.));
#12124=DIRECTION('ref_axis',(1.,0.,0.));
#12125=DIRECTION('',(0.,-1.,0.));
#12126=DIRECTION('center_axis',(0.,-1.,0.));
#12127=DIRECTION('ref_axis',(1.,0.,0.));
#12128=DIRECTION('center_axis',(0.,1.,0.));
#12129=DIRECTION('ref_axis',(1.,0.,0.));
#12130=DIRECTION('center_axis',(0.,1.,0.));
#12131=DIRECTION('ref_axis',(1.,0.,0.));
#12132=DIRECTION('',(0.,-1.,0.));
#12133=DIRECTION('center_axis',(0.,1.,0.));
#12134=DIRECTION('ref_axis',(1.,0.,0.));
#12135=DIRECTION('center_axis',(0.,1.,0.));
#12136=DIRECTION('ref_axis',(1.,0.,0.));
#12137=DIRECTION('center_axis',(0.,1.,0.));
#12138=DIRECTION('ref_axis',(1.,0.,0.));
#12139=DIRECTION('axis',(0.,0.,1.));
#12140=DIRECTION('refdir',(1.,0.,0.));
#12141=DIRECTION('center_axis',(0.,1.,0.));
#12142=DIRECTION('ref_axis',(1.,0.,0.));
#12143=DIRECTION('center_axis',(0.,-1.,0.));
#12144=DIRECTION('ref_axis',(1.,0.,0.));
#12145=DIRECTION('',(0.,-1.,0.));
#12146=DIRECTION('center_axis',(0.,-1.,0.));
#12147=DIRECTION('ref_axis',(1.,0.,0.));
#12148=DIRECTION('center_axis',(0.,1.,0.));
#12149=DIRECTION('ref_axis',(1.,0.,0.));
#12150=DIRECTION('center_axis',(0.,1.,0.));
#12151=DIRECTION('ref_axis',(1.,0.,0.));
#12152=DIRECTION('',(0.,-1.,0.));
#12153=DIRECTION('center_axis',(0.,1.,0.));
#12154=DIRECTION('ref_axis',(1.,0.,0.));
#12155=DIRECTION('center_axis',(0.,1.,0.));
#12156=DIRECTION('ref_axis',(1.,0.,0.));
#12157=DIRECTION('center_axis',(0.,1.,0.));
#12158=DIRECTION('ref_axis',(1.,0.,0.));
#12159=DIRECTION('axis',(0.,0.,1.));
#12160=DIRECTION('refdir',(1.,0.,0.));
#12161=DIRECTION('center_axis',(0.,1.,0.));
#12162=DIRECTION('ref_axis',(1.,0.,0.));
#12163=DIRECTION('center_axis',(0.,-1.,0.));
#12164=DIRECTION('ref_axis',(1.,0.,0.));
#12165=DIRECTION('',(0.,-1.,0.));
#12166=DIRECTION('center_axis',(0.,-1.,0.));
#12167=DIRECTION('ref_axis',(1.,0.,0.));
#12168=DIRECTION('center_axis',(0.,1.,0.));
#12169=DIRECTION('ref_axis',(1.,0.,0.));
#12170=DIRECTION('center_axis',(0.,1.,0.));
#12171=DIRECTION('ref_axis',(1.,0.,0.));
#12172=DIRECTION('',(0.,-1.,0.));
#12173=DIRECTION('center_axis',(0.,1.,0.));
#12174=DIRECTION('ref_axis',(1.,0.,0.));
#12175=DIRECTION('center_axis',(0.,1.,0.));
#12176=DIRECTION('ref_axis',(1.,0.,0.));
#12177=DIRECTION('center_axis',(0.,1.,0.));
#12178=DIRECTION('ref_axis',(1.,0.,0.));
#12179=DIRECTION('axis',(0.,0.,1.));
#12180=DIRECTION('refdir',(1.,0.,0.));
#12181=DIRECTION('axis',(0.,0.,1.));
#12182=DIRECTION('refdir',(1.,0.,0.));
#12183=DIRECTION('center_axis',(0.,-1.,0.));
#12184=DIRECTION('ref_axis',(0.,0.,-1.));
#12185=DIRECTION('center_axis',(0.,-1.,0.));
#12186=DIRECTION('ref_axis',(1.,0.,0.));
#12187=DIRECTION('center_axis',(0.,-1.,0.));
#12188=DIRECTION('ref_axis',(1.,0.,0.));
#12189=DIRECTION('center_axis',(1.,0.,1.22464679914735E-16));
#12190=DIRECTION('ref_axis',(-1.22464679914735E-16,0.,1.));
#12191=DIRECTION('center_axis',(0.,1.,0.));
#12192=DIRECTION('ref_axis',(1.,0.,0.));
#12193=DIRECTION('center_axis',(0.,1.,0.));
#12194=DIRECTION('ref_axis',(1.,0.,0.));
#12195=DIRECTION('center_axis',(0.,-1.,0.));
#12196=DIRECTION('ref_axis',(1.,0.,0.));
#12197=DIRECTION('',(0.,1.,0.));
#12198=DIRECTION('center_axis',(0.,-1.,0.));
#12199=DIRECTION('ref_axis',(1.,0.,0.));
#12200=DIRECTION('center_axis',(0.,-1.,0.));
#12201=DIRECTION('ref_axis',(1.,0.,0.));
#12202=DIRECTION('center_axis',(0.,-1.,0.));
#12203=DIRECTION('ref_axis',(1.,0.,0.));
#12204=DIRECTION('',(0.,1.,0.));
#12205=DIRECTION('center_axis',(0.,-1.,0.));
#12206=DIRECTION('ref_axis',(1.,0.,0.));
#12207=DIRECTION('center_axis',(0.,1.,0.));
#12208=DIRECTION('ref_axis',(1.,0.,0.));
#12209=DIRECTION('',(-0.707106781186547,0.707106781186548,-8.65956056235493E-17));
#12210=DIRECTION('center_axis',(0.,-1.,0.));
#12211=DIRECTION('ref_axis',(1.,0.,0.));
#12212=DIRECTION('center_axis',(0.,1.,0.));
#12213=DIRECTION('ref_axis',(0.,0.,1.));
#12214=DIRECTION('center_axis',(0.,-1.,0.));
#12215=DIRECTION('ref_axis',(1.,0.,0.));
#12216=DIRECTION('center_axis',(0.,-1.,0.));
#12217=DIRECTION('ref_axis',(1.,0.,0.));
#12218=DIRECTION('',(0.,1.,0.));
#12219=DIRECTION('center_axis',(0.,-1.,0.));
#12220=DIRECTION('ref_axis',(0.,0.,-1.));
#12221=DIRECTION('center_axis',(0.,-1.,0.));
#12222=DIRECTION('ref_axis',(1.,0.,0.));
#12223=DIRECTION('center_axis',(0.,-1.,0.));
#12224=DIRECTION('ref_axis',(1.,0.,0.));
#12225=DIRECTION('',(0.707106781186547,0.707106781186548,8.65956056235493E-17));
#12226=DIRECTION('axis',(0.,0.,1.));
#12227=DIRECTION('refdir',(1.,0.,0.));
#12228=DIRECTION('center_axis',(0.,-1.,0.));
#12229=DIRECTION('ref_axis',(0.,0.,-1.));
#12230=DIRECTION('center_axis',(0.,-1.,0.));
#12231=DIRECTION('ref_axis',(1.,0.,0.));
#12232=DIRECTION('center_axis',(0.,-1.,0.));
#12233=DIRECTION('ref_axis',(1.,0.,0.));
#12234=DIRECTION('center_axis',(1.,0.,1.22464679914735E-16));
#12235=DIRECTION('ref_axis',(-1.22464679914735E-16,0.,1.));
#12236=DIRECTION('center_axis',(0.,1.,0.));
#12237=DIRECTION('ref_axis',(1.,0.,0.));
#12238=DIRECTION('center_axis',(0.,1.,0.));
#12239=DIRECTION('ref_axis',(1.,0.,0.));
#12240=DIRECTION('center_axis',(0.,-1.,0.));
#12241=DIRECTION('ref_axis',(1.,0.,0.));
#12242=DIRECTION('center_axis',(0.,-1.,0.));
#12243=DIRECTION('ref_axis',(1.,0.,0.));
#12244=DIRECTION('',(0.,1.,0.));
#12245=DIRECTION('center_axis',(0.,1.,0.));
#12246=DIRECTION('ref_axis',(0.,0.,1.));
#12247=DIRECTION('center_axis',(0.,-1.,0.));
#12248=DIRECTION('ref_axis',(1.,0.,0.));
#12249=DIRECTION('center_axis',(0.,-1.,0.));
#12250=DIRECTION('ref_axis',(1.,0.,0.));
#12251=DIRECTION('center_axis',(0.,-1.,0.));
#12252=DIRECTION('ref_axis',(1.,0.,0.));
#12253=DIRECTION('center_axis',(0.,-1.,0.));
#12254=DIRECTION('ref_axis',(1.,0.,0.));
#12255=DIRECTION('',(0.707106781186548,0.707106781186547,8.65956056235494E-17));
#12256=DIRECTION('center_axis',(0.,-1.,0.));
#12257=DIRECTION('ref_axis',(1.,0.,0.));
#12258=DIRECTION('center_axis',(0.,-1.,0.));
#12259=DIRECTION('ref_axis',(1.,0.,0.));
#12260=DIRECTION('',(0.,1.,0.));
#12261=DIRECTION('center_axis',(0.,1.,0.));
#12262=DIRECTION('ref_axis',(1.,0.,0.));
#12263=DIRECTION('center_axis',(0.,-1.,0.));
#12264=DIRECTION('ref_axis',(1.,0.,0.));
#12265=DIRECTION('',(-0.707106781186548,0.707106781186547,-8.65956056235494E-17));
#12266=DIRECTION('center_axis',(0.,-1.,0.));
#12267=DIRECTION('ref_axis',(0.,0.,-1.));
#12268=DIRECTION('center_axis',(0.,-1.,0.));
#12269=DIRECTION('ref_axis',(1.,0.,0.));
#12270=DIRECTION('',(0.,1.,0.));
#12271=DIRECTION('axis',(0.,0.,1.));
#12272=DIRECTION('refdir',(1.,0.,0.));
#12273=DIRECTION('center_axis',(0.,0.,1.));
#12274=DIRECTION('ref_axis',(1.,0.,0.));
#12275=DIRECTION('center_axis',(1.22464679914735E-16,-1.,0.));
#12276=DIRECTION('ref_axis',(-1.,-1.22464679914735E-16,0.));
#12277=DIRECTION('center_axis',(0.707106781186548,0.,0.707106781186548));
#12278=DIRECTION('ref_axis',(0.707106781186548,0.,-0.707106781186548));
#12279=DIRECTION('center_axis',(8.65956056235494E-17,-1.,-8.65956056235493E-17));
#12280=DIRECTION('ref_axis',(-0.707106781186547,-1.22464679914735E-16,0.707106781186547));
#12281=DIRECTION('center_axis',(1.,0.,0.));
#12282=DIRECTION('ref_axis',(6.12323399573676E-17,0.,-1.));
#12283=DIRECTION('center_axis',(7.49879891330929E-33,-1.,-1.22464679914735E-16));
#12284=DIRECTION('ref_axis',(-6.12323399573676E-17,-1.22464679914735E-16,
1.));
#12285=DIRECTION('center_axis',(0.707106781186548,0.,-0.707106781186548));
#12286=DIRECTION('ref_axis',(-0.707106781186548,0.,-0.707106781186548));
#12287=DIRECTION('center_axis',(-8.65956056235493E-17,-1.,-8.65956056235494E-17));
#12288=DIRECTION('ref_axis',(0.707106781186547,-1.22464679914735E-16,0.707106781186547));
#12289=DIRECTION('center_axis',(0.,0.,-1.));
#12290=DIRECTION('ref_axis',(-1.,0.,-1.22464679914735E-16));
#12291=DIRECTION('center_axis',(-1.22464679914735E-16,-1.,-1.49975978266186E-32));
#12292=DIRECTION('ref_axis',(1.,-1.22464679914735E-16,1.22464679914735E-16));
#12293=DIRECTION('center_axis',(-0.707106781186547,0.,-0.707106781186548));
#12294=DIRECTION('ref_axis',(-0.707106781186548,0.,0.707106781186547));
#12295=DIRECTION('center_axis',(-8.65956056235493E-17,-1.,8.65956056235493E-17));
#12296=DIRECTION('ref_axis',(0.707106781186548,-1.22464679914735E-16,-0.707106781186547));
#12297=DIRECTION('center_axis',(-1.,0.,0.));
#12298=DIRECTION('ref_axis',(-1.83697019872103E-16,0.,1.));
#12299=DIRECTION('center_axis',(-2.24963967399279E-32,-1.,1.22464679914735E-16));
#12300=DIRECTION('ref_axis',(1.83697019872103E-16,-1.22464679914735E-16,
-1.));
#12301=DIRECTION('center_axis',(-0.707106781186548,0.,0.707106781186548));
#12302=DIRECTION('ref_axis',(0.707106781186547,0.,0.707106781186548));
#12303=DIRECTION('center_axis',(8.65956056235493E-17,-1.,8.65956056235493E-17));
#12304=DIRECTION('ref_axis',(-0.707106781186547,-1.22464679914735E-16,-0.707106781186548));
#12305=DIRECTION('axis',(0.,0.,1.));
#12306=DIRECTION('refdir',(1.,0.,0.));
#12307=DIRECTION('center_axis',(0.,0.,1.));
#12308=DIRECTION('ref_axis',(1.,0.,0.));
#12309=DIRECTION('center_axis',(0.,-1.,0.));
#12310=DIRECTION('ref_axis',(0.,0.,-1.));
#12311=DIRECTION('center_axis',(0.,-1.,0.));
#12312=DIRECTION('ref_axis',(0.,0.,-1.));
#12313=DIRECTION('center_axis',(0.,1.,0.));
#12314=DIRECTION('ref_axis',(1.,0.,0.));
#12315=DIRECTION('center_axis',(0.,1.,0.));
#12316=DIRECTION('ref_axis',(1.,0.,0.));
#12317=DIRECTION('center_axis',(0.,1.,0.));
#12318=DIRECTION('ref_axis',(1.,0.,0.));
#12319=DIRECTION('center_axis',(0.,1.,0.));
#12320=DIRECTION('ref_axis',(1.,0.,0.));
#12321=DIRECTION('',(0.,-1.,0.));
#12322=DIRECTION('center_axis',(0.,-1.,0.));
#12323=DIRECTION('ref_axis',(1.,0.,0.));
#12324=DIRECTION('center_axis',(0.,1.,0.));
#12325=DIRECTION('ref_axis',(1.,0.,0.));
#12326=DIRECTION('center_axis',(0.,1.,0.));
#12327=DIRECTION('ref_axis',(1.,0.,0.));
#12328=DIRECTION('center_axis',(0.,1.,0.));
#12329=DIRECTION('ref_axis',(1.,0.,0.));
#12330=DIRECTION('center_axis',(0.,1.,0.));
#12331=DIRECTION('ref_axis',(1.,0.,0.));
#12332=DIRECTION('center_axis',(0.,1.,0.));
#12333=DIRECTION('ref_axis',(1.,0.,0.));
#12334=DIRECTION('center_axis',(0.,1.,0.));
#12335=DIRECTION('ref_axis',(1.,0.,0.));
#12336=DIRECTION('center_axis',(0.,-1.,0.));
#12337=DIRECTION('ref_axis',(1.,0.,0.));
#12338=DIRECTION('center_axis',(0.,-1.,0.));
#12339=DIRECTION('ref_axis',(0.,0.,-1.));
#12340=DIRECTION('center_axis',(6.12323399573677E-17,0.,1.));
#12341=DIRECTION('ref_axis',(1.,0.,0.));
#12342=DIRECTION('center_axis',(0.,-1.,0.));
#12343=DIRECTION('ref_axis',(0.,0.,-1.));
#12344=DIRECTION('center_axis',(0.,1.,0.));
#12345=DIRECTION('ref_axis',(1.,0.,0.));
#12346=DIRECTION('center_axis',(0.,-1.,0.));
#12347=DIRECTION('ref_axis',(1.,0.,0.));
#12348=DIRECTION('center_axis',(0.,-1.,0.));
#12349=DIRECTION('ref_axis',(0.,0.,-1.));
#12350=DIRECTION('center_axis',(0.,0.,1.));
#12351=DIRECTION('ref_axis',(1.,0.,0.));
#12352=DIRECTION('center_axis',(0.,-1.,0.));
#12353=DIRECTION('ref_axis',(0.,0.,-1.));
#12354=DIRECTION('center_axis',(0.,1.,0.));
#12355=DIRECTION('ref_axis',(1.,0.,0.));
#12356=DIRECTION('center_axis',(0.,-1.,0.));
#12357=DIRECTION('ref_axis',(1.,0.,0.));
#12358=DIRECTION('center_axis',(0.,-1.,0.));
#12359=DIRECTION('ref_axis',(0.,0.,-1.));
#12360=DIRECTION('center_axis',(0.,0.,1.));
#12361=DIRECTION('ref_axis',(1.,0.,0.));
#12362=DIRECTION('center_axis',(0.,-1.,0.));
#12363=DIRECTION('ref_axis',(0.,0.,-1.));
#12364=DIRECTION('center_axis',(0.,1.,0.));
#12365=DIRECTION('ref_axis',(1.,0.,0.));
#12366=DIRECTION('center_axis',(0.,-1.,0.));
#12367=DIRECTION('ref_axis',(1.,0.,0.));
#12368=DIRECTION('center_axis',(0.,-1.,0.));
#12369=DIRECTION('ref_axis',(0.,0.,-1.));
#12370=DIRECTION('center_axis',(0.,0.,1.));
#12371=DIRECTION('ref_axis',(1.,0.,0.));
#12372=DIRECTION('center_axis',(0.,-1.,0.));
#12373=DIRECTION('ref_axis',(0.,0.,-1.));
#12374=DIRECTION('center_axis',(0.,1.,0.));
#12375=DIRECTION('ref_axis',(1.,0.,0.));
#12376=DIRECTION('center_axis',(0.,-1.,0.));
#12377=DIRECTION('ref_axis',(1.,0.,0.));
#12378=DIRECTION('center_axis',(0.,-1.,0.));
#12379=DIRECTION('ref_axis',(0.,0.,-1.));
#12380=DIRECTION('center_axis',(6.12323399573676E-17,0.,1.));
#12381=DIRECTION('ref_axis',(1.,0.,0.));
#12382=DIRECTION('center_axis',(0.,-1.,0.));
#12383=DIRECTION('ref_axis',(0.,0.,-1.));
#12384=DIRECTION('center_axis',(0.,1.,0.));
#12385=DIRECTION('ref_axis',(1.,0.,0.));
#12386=DIRECTION('center_axis',(0.,-1.,0.));
#12387=DIRECTION('ref_axis',(1.,0.,0.));
#12388=DIRECTION('center_axis',(0.,-1.,0.));
#12389=DIRECTION('ref_axis',(0.,0.,-1.));
#12390=DIRECTION('center_axis',(0.,0.,1.));
#12391=DIRECTION('ref_axis',(1.,0.,0.));
#12392=DIRECTION('center_axis',(0.,-1.,0.));
#12393=DIRECTION('ref_axis',(0.,0.,-1.));
#12394=DIRECTION('center_axis',(0.,1.,0.));
#12395=DIRECTION('ref_axis',(1.,0.,0.));
#12396=DIRECTION('center_axis',(0.,1.,0.));
#12397=DIRECTION('ref_axis',(1.,0.,0.));
#12398=DIRECTION('',(0.,1.,0.));
#12399=DIRECTION('center_axis',(0.,-1.,0.));
#12400=DIRECTION('ref_axis',(1.,0.,0.));
#12401=DIRECTION('center_axis',(0.,-1.,0.));
#12402=DIRECTION('ref_axis',(1.,0.,0.));
#12403=DIRECTION('center_axis',(0.,1.,0.));
#12404=DIRECTION('ref_axis',(1.,0.,0.));
#12405=DIRECTION('center_axis',(0.,-1.,0.));
#12406=DIRECTION('ref_axis',(0.,0.,-1.));
#12407=DIRECTION('center_axis',(0.,0.,1.));
#12408=DIRECTION('ref_axis',(1.,0.,0.));
#12409=DIRECTION('center_axis',(0.,-1.,0.));
#12410=DIRECTION('ref_axis',(0.,0.,-1.));
#12411=DIRECTION('center_axis',(0.,-1.,0.));
#12412=DIRECTION('ref_axis',(-1.,0.,0.));
#12413=DIRECTION('center_axis',(0.,1.,0.));
#12414=DIRECTION('ref_axis',(1.,0.,0.));
#12415=DIRECTION('axis',(0.,0.,1.));
#12416=DIRECTION('refdir',(1.,0.,0.));
#12417=DIRECTION('center_axis',(0.,1.,0.));
#12418=DIRECTION('ref_axis',(0.,0.,1.));
#12419=DIRECTION('center_axis',(0.,-1.,0.));
#12420=DIRECTION('ref_axis',(1.,0.,0.));
#12421=DIRECTION('center_axis',(0.,-1.,0.));
#12422=DIRECTION('ref_axis',(1.,0.,0.));
#12423=DIRECTION('center_axis',(0.,-1.,0.));
#12424=DIRECTION('ref_axis',(1.,0.,0.));
#12425=DIRECTION('center_axis',(0.,-1.,0.));
#12426=DIRECTION('ref_axis',(1.,0.,0.));
#12427=DIRECTION('',(0.,1.,0.));
#12428=DIRECTION('center_axis',(0.,-1.,0.));
#12429=DIRECTION('ref_axis',(0.,0.,-1.));
#12430=DIRECTION('center_axis',(0.,-1.,0.));
#12431=DIRECTION('ref_axis',(1.,0.,0.));
#12432=DIRECTION('center_axis',(0.,-1.,0.));
#12433=DIRECTION('ref_axis',(1.,0.,0.));
#12434=DIRECTION('',(0.,1.,0.));
#12435=DIRECTION('center_axis',(0.,1.,0.));
#12436=DIRECTION('ref_axis',(0.,0.,1.));
#12437=DIRECTION('center_axis',(0.,-1.,0.));
#12438=DIRECTION('ref_axis',(1.,0.,0.));
#12439=DIRECTION('center_axis',(0.,-1.,0.));
#12440=DIRECTION('ref_axis',(1.,0.,0.));
#12441=DIRECTION('center_axis',(0.,-1.,0.));
#12442=DIRECTION('ref_axis',(1.,0.,0.));
#12443=DIRECTION('center_axis',(0.,-1.,0.));
#12444=DIRECTION('ref_axis',(1.,0.,0.));
#12445=DIRECTION('',(0.,1.,0.));
#12446=DIRECTION('center_axis',(0.,-1.,0.));
#12447=DIRECTION('ref_axis',(0.,0.,-1.));
#12448=DIRECTION('center_axis',(0.,-1.,0.));
#12449=DIRECTION('ref_axis',(1.,0.,0.));
#12450=DIRECTION('center_axis',(0.,-1.,0.));
#12451=DIRECTION('ref_axis',(1.,0.,0.));
#12452=DIRECTION('',(0.,1.,0.));
#12453=DIRECTION('',(0.,0.,1.));
#12454=DIRECTION('',(1.,0.,0.));
#12455=DIRECTION('',(0.,0.,1.));
#12456=DIRECTION('',(1.,0.,0.));
#12457=DIRECTION('',(0.,0.,1.));
#12458=DIRECTION('',(1.,0.,0.));
#12459=DIRECTION('',(0.,0.,1.));
#12460=DIRECTION('',(1.,0.,0.));
#12461=DIRECTION('',(0.,0.,1.));
#12462=DIRECTION('',(1.,0.,0.));
#12463=DIRECTION('',(0.,0.,1.));
#12464=DIRECTION('',(1.,0.,0.));
#12465=DIRECTION('',(0.,0.,1.));
#12466=DIRECTION('',(1.,0.,0.));
#12467=DIRECTION('',(0.,0.,1.));
#12468=DIRECTION('',(1.,0.,0.));
#12469=DIRECTION('',(0.,0.,1.));
#12470=DIRECTION('',(1.,0.,0.));
#12471=DIRECTION('',(0.,0.,1.));
#12472=DIRECTION('',(1.,0.,0.));
#12473=DIRECTION('',(0.,0.,1.));
#12474=DIRECTION('',(1.,0.,0.));
#12475=DIRECTION('',(0.,0.,1.));
#12476=DIRECTION('',(1.,0.,0.));
#12477=DIRECTION('axis',(0.,0.,1.));
#12478=DIRECTION('refdir',(1.,0.,0.));
#12479=DIRECTION('axis',(0.,0.,1.));
#12480=DIRECTION('refdir',(1.,0.,0.));
#12481=DIRECTION('center_axis',(0.,0.,1.));
#12482=DIRECTION('ref_axis',(1.,0.,0.));
#12483=DIRECTION('center_axis',(0.,0.,1.));
#12484=DIRECTION('ref_axis',(1.,0.,0.));
#12485=DIRECTION('',(0.,0.,1.));
#12486=DIRECTION('center_axis',(0.,0.,-1.));
#12487=DIRECTION('ref_axis',(1.,0.,0.));
#12488=DIRECTION('center_axis',(0.,0.,1.));
#12489=DIRECTION('ref_axis',(1.,0.,0.));
#12490=DIRECTION('center_axis',(0.,0.,1.));
#12491=DIRECTION('ref_axis',(1.,0.,0.));
#12492=DIRECTION('center_axis',(0.,0.,1.));
#12493=DIRECTION('ref_axis',(1.,0.,0.));
#12494=DIRECTION('',(0.,0.,1.));
#12495=DIRECTION('center_axis',(0.,0.,-1.));
#12496=DIRECTION('ref_axis',(1.,0.,0.));
#12497=DIRECTION('center_axis',(0.,0.,1.));
#12498=DIRECTION('ref_axis',(1.,0.,0.));
#12499=DIRECTION('center_axis',(-1.,0.,0.));
#12500=DIRECTION('ref_axis',(0.,0.,1.));
#12501=DIRECTION('',(0.,0.,-1.));
#12502=DIRECTION('',(0.,1.,0.));
#12503=DIRECTION('',(0.,0.,1.));
#12504=DIRECTION('',(0.,1.,0.));
#12505=DIRECTION('center_axis',(1.,0.,0.));
#12506=DIRECTION('ref_axis',(0.,0.,-1.));
#12507=DIRECTION('',(0.,0.,1.));
#12508=DIRECTION('',(0.,-1.,0.));
#12509=DIRECTION('',(0.,0.,-1.));
#12510=DIRECTION('',(0.,1.,0.));
#12511=DIRECTION('center_axis',(0.,0.,1.));
#12512=DIRECTION('ref_axis',(1.,0.,0.));
#12513=DIRECTION('',(-1.,0.,0.));
#12514=DIRECTION('',(1.,0.,0.));
#12515=DIRECTION('center_axis',(0.,1.,0.));
#12516=DIRECTION('ref_axis',(0.,0.,1.));
#12517=DIRECTION('',(1.,0.,0.));
#12518=DIRECTION('center_axis',(0.,1.,0.));
#12519=DIRECTION('ref_axis',(1.,0.,0.));
#12520=DIRECTION('center_axis',(0.,1.,0.));
#12521=DIRECTION('ref_axis',(1.,0.,0.));
#12522=DIRECTION('',(0.,1.,0.));
#12523=DIRECTION('center_axis',(0.,-1.,0.));
#12524=DIRECTION('ref_axis',(1.,0.,0.));
#12525=DIRECTION('center_axis',(0.,1.,0.));
#12526=DIRECTION('ref_axis',(1.,0.,0.));
#12527=DIRECTION('',(-1.,0.,0.));
#12528=DIRECTION('',(0.,0.,1.));
#12529=DIRECTION('',(-1.,0.,0.));
#12530=DIRECTION('',(0.,0.,-1.));
#12531=DIRECTION('center_axis',(1.,0.,0.));
#12532=DIRECTION('ref_axis',(0.,0.,-1.));
#12533=DIRECTION('',(0.,-1.,0.));
#12534=DIRECTION('',(0.,0.,-1.));
#12535=DIRECTION('',(0.,1.,0.));
#12536=DIRECTION('center_axis',(-1.,0.,0.));
#12537=DIRECTION('ref_axis',(0.,0.,1.));
#12538=DIRECTION('',(0.,1.,0.));
#12539=DIRECTION('',(0.,1.,0.));
#12540=DIRECTION('',(0.,0.,1.));
#12541=DIRECTION('center_axis',(0.,0.,1.));
#12542=DIRECTION('ref_axis',(1.,0.,0.));
#12543=DIRECTION('',(1.,0.,0.));
#12544=DIRECTION('center_axis',(0.,1.,0.));
#12545=DIRECTION('ref_axis',(0.,0.,1.));
#12546=DIRECTION('',(1.,0.,0.));
#12547=DIRECTION('center_axis',(0.,0.,1.));
#12548=DIRECTION('ref_axis',(1.,0.,0.));
#12549=DIRECTION('center_axis',(0.,0.,1.));
#12550=DIRECTION('ref_axis',(1.,0.,0.));
#12551=DIRECTION('',(0.,0.,1.));
#12552=DIRECTION('center_axis',(0.,0.,-1.));
#12553=DIRECTION('ref_axis',(1.,0.,0.));
#12554=DIRECTION('center_axis',(0.,0.,1.));
#12555=DIRECTION('ref_axis',(1.,0.,0.));
#12556=DIRECTION('center_axis',(0.,0.,1.));
#12557=DIRECTION('ref_axis',(1.,0.,0.));
#12558=DIRECTION('',(0.,0.,1.));
#12559=DIRECTION('center_axis',(0.,0.,-1.));
#12560=DIRECTION('ref_axis',(1.,0.,0.));
#12561=DIRECTION('center_axis',(0.,0.,1.));
#12562=DIRECTION('ref_axis',(1.,0.,0.));
#12563=DIRECTION('center_axis',(0.,0.,1.));
#12564=DIRECTION('ref_axis',(1.,0.,0.));
#12565=DIRECTION('',(0.,0.,1.));
#12566=DIRECTION('center_axis',(0.,0.,-1.));
#12567=DIRECTION('ref_axis',(1.,0.,0.));
#12568=DIRECTION('center_axis',(0.,0.,1.));
#12569=DIRECTION('ref_axis',(1.,0.,0.));
#12570=DIRECTION('center_axis',(0.,0.,1.));
#12571=DIRECTION('ref_axis',(1.,0.,0.));
#12572=DIRECTION('',(0.,0.,1.));
#12573=DIRECTION('center_axis',(0.,0.,-1.));
#12574=DIRECTION('ref_axis',(1.,0.,0.));
#12575=DIRECTION('center_axis',(0.,1.,0.));
#12576=DIRECTION('ref_axis',(-1.,0.,0.));
#12577=DIRECTION('',(-1.,0.,0.));
#12578=DIRECTION('',(0.,0.,1.));
#12579=DIRECTION('',(-1.,0.,0.));
#12580=DIRECTION('',(0.,0.,1.));
#12581=DIRECTION('center_axis',(1.,0.,0.));
#12582=DIRECTION('ref_axis',(0.,1.,0.));
#12583=DIRECTION('',(0.,1.,0.));
#12584=DIRECTION('',(0.,1.,0.));
#12585=DIRECTION('',(0.,0.,1.));
#12586=DIRECTION('center_axis',(0.,-1.,0.));
#12587=DIRECTION('ref_axis',(1.,0.,0.));
#12588=DIRECTION('',(1.,0.,0.));
#12589=DIRECTION('',(1.,0.,0.));
#12590=DIRECTION('',(1.,0.,0.));
#12591=DIRECTION('',(0.,0.,1.));
#12592=DIRECTION('center_axis',(-1.,0.,0.));
#12593=DIRECTION('ref_axis',(0.,-1.,0.));
#12594=DIRECTION('',(0.,-1.,0.));
#12595=DIRECTION('',(0.,-1.,0.));
#12596=DIRECTION('center_axis',(0.,0.,1.));
#12597=DIRECTION('ref_axis',(1.,0.,0.));
#12598=DIRECTION('center_axis',(0.,0.,1.));
#12599=DIRECTION('ref_axis',(1.,0.,0.));
#12600=DIRECTION('axis',(0.,0.,1.));
#12601=DIRECTION('refdir',(1.,0.,0.));
#12602=DIRECTION('center_axis',(0.,0.,1.));
#12603=DIRECTION('ref_axis',(1.,0.,0.));
#12604=DIRECTION('center_axis',(0.,0.,1.));
#12605=DIRECTION('ref_axis',(1.,0.,0.));
#12606=DIRECTION('',(0.,0.,1.));
#12607=DIRECTION('center_axis',(0.,0.,-1.));
#12608=DIRECTION('ref_axis',(1.,0.,0.));
#12609=DIRECTION('center_axis',(0.,0.,1.));
#12610=DIRECTION('ref_axis',(1.,0.,0.));
#12611=DIRECTION('center_axis',(0.,0.,1.));
#12612=DIRECTION('ref_axis',(1.,0.,0.));
#12613=DIRECTION('',(0.,0.,1.));
#12614=DIRECTION('center_axis',(0.,0.,-1.));
#12615=DIRECTION('ref_axis',(1.,0.,0.));
#12616=DIRECTION('center_axis',(0.,1.,0.));
#12617=DIRECTION('ref_axis',(-1.,0.,0.));
#12618=DIRECTION('',(-1.,0.,0.));
#12619=DIRECTION('',(0.,0.,1.));
#12620=DIRECTION('',(-1.,0.,0.));
#12621=DIRECTION('',(0.,0.,1.));
#12622=DIRECTION('center_axis',(1.,0.,0.));
#12623=DIRECTION('ref_axis',(0.,1.,0.));
#12624=DIRECTION('',(0.,1.,0.));
#12625=DIRECTION('',(0.,1.,0.));
#12626=DIRECTION('',(0.,0.,1.));
#12627=DIRECTION('center_axis',(0.,-1.,0.));
#12628=DIRECTION('ref_axis',(1.,0.,0.));
#12629=DIRECTION('',(1.,0.,0.));
#12630=DIRECTION('',(1.,0.,0.));
#12631=DIRECTION('',(0.,0.,1.));
#12632=DIRECTION('center_axis',(-1.,0.,0.));
#12633=DIRECTION('ref_axis',(0.,-1.,0.));
#12634=DIRECTION('',(0.,-1.,0.));
#12635=DIRECTION('',(0.,-1.,0.));
#12636=DIRECTION('center_axis',(0.,0.,1.));
#12637=DIRECTION('ref_axis',(1.,0.,0.));
#12638=DIRECTION('center_axis',(0.,0.,1.));
#12639=DIRECTION('ref_axis',(1.,0.,0.));
#12640=DIRECTION('axis',(0.,0.,1.));
#12641=DIRECTION('refdir',(1.,0.,0.));
#12642=DIRECTION('center_axis',(0.,1.,0.));
#12643=DIRECTION('ref_axis',(1.,0.,0.));
#12644=DIRECTION('center_axis',(0.,1.,0.));
#12645=DIRECTION('ref_axis',(1.,0.,0.));
#12646=DIRECTION('',(0.,1.,0.));
#12647=DIRECTION('center_axis',(0.,-1.,0.));
#12648=DIRECTION('ref_axis',(1.,0.,0.));
#12649=DIRECTION('center_axis',(0.,1.,0.));
#12650=DIRECTION('ref_axis',(1.,0.,0.));
#12651=DIRECTION('center_axis',(0.,1.,0.));
#12652=DIRECTION('ref_axis',(1.,0.,0.));
#12653=DIRECTION('center_axis',(0.,1.,0.));
#12654=DIRECTION('ref_axis',(1.,0.,0.));
#12655=DIRECTION('center_axis',(0.,1.,0.));
#12656=DIRECTION('ref_axis',(1.,0.,0.));
#12657=DIRECTION('center_axis',(0.,1.,0.));
#12658=DIRECTION('ref_axis',(1.,0.,0.));
#12659=DIRECTION('',(0.,-1.,0.));
#12660=DIRECTION('center_axis',(0.,1.,0.));
#12661=DIRECTION('ref_axis',(1.,0.,0.));
#12662=DIRECTION('center_axis',(0.,1.,0.));
#12663=DIRECTION('ref_axis',(1.,0.,0.));
#12664=DIRECTION('center_axis',(0.,1.,0.));
#12665=DIRECTION('ref_axis',(1.,0.,0.));
#12666=DIRECTION('center_axis',(0.,1.,0.));
#12667=DIRECTION('ref_axis',(1.,0.,0.));
#12668=DIRECTION('',(0.,-1.,0.));
#12669=DIRECTION('center_axis',(0.,1.,0.));
#12670=DIRECTION('ref_axis',(1.,0.,0.));
#12671=DIRECTION('axis',(0.,0.,1.));
#12672=DIRECTION('refdir',(1.,0.,0.));
#12673=DIRECTION('center_axis',(0.,1.,0.));
#12674=DIRECTION('ref_axis',(1.,0.,0.));
#12675=DIRECTION('center_axis',(0.,-1.,0.));
#12676=DIRECTION('ref_axis',(1.,0.,0.));
#12677=DIRECTION('',(0.,-1.,0.));
#12678=DIRECTION('center_axis',(0.,-1.,0.));
#12679=DIRECTION('ref_axis',(1.,0.,0.));
#12680=DIRECTION('center_axis',(0.,1.,0.));
#12681=DIRECTION('ref_axis',(1.,0.,0.));
#12682=DIRECTION('center_axis',(0.,1.,0.));
#12683=DIRECTION('ref_axis',(1.,0.,0.));
#12684=DIRECTION('',(0.,-1.,0.));
#12685=DIRECTION('center_axis',(0.,1.,0.));
#12686=DIRECTION('ref_axis',(1.,0.,0.));
#12687=DIRECTION('center_axis',(0.,1.,0.));
#12688=DIRECTION('ref_axis',(1.,0.,0.));
#12689=DIRECTION('center_axis',(0.,1.,0.));
#12690=DIRECTION('ref_axis',(1.,0.,0.));
#12691=DIRECTION('axis',(0.,0.,1.));
#12692=DIRECTION('refdir',(1.,0.,0.));
#12693=DIRECTION('center_axis',(0.,1.,0.));
#12694=DIRECTION('ref_axis',(1.,0.,0.));
#12695=DIRECTION('center_axis',(0.,-1.,0.));
#12696=DIRECTION('ref_axis',(1.,0.,0.));
#12697=DIRECTION('',(0.,-1.,0.));
#12698=DIRECTION('center_axis',(0.,-1.,0.));
#12699=DIRECTION('ref_axis',(1.,0.,0.));
#12700=DIRECTION('center_axis',(0.,1.,0.));
#12701=DIRECTION('ref_axis',(1.,0.,0.));
#12702=DIRECTION('center_axis',(0.,1.,0.));
#12703=DIRECTION('ref_axis',(1.,0.,0.));
#12704=DIRECTION('',(0.,-1.,0.));
#12705=DIRECTION('center_axis',(0.,1.,0.));
#12706=DIRECTION('ref_axis',(1.,0.,0.));
#12707=DIRECTION('center_axis',(0.,1.,0.));
#12708=DIRECTION('ref_axis',(1.,0.,0.));
#12709=DIRECTION('center_axis',(0.,1.,0.));
#12710=DIRECTION('ref_axis',(1.,0.,0.));
#12711=DIRECTION('axis',(0.,0.,1.));
#12712=DIRECTION('refdir',(1.,0.,0.));
#12713=DIRECTION('center_axis',(0.,1.,0.));
#12714=DIRECTION('ref_axis',(1.,0.,0.));
#12715=DIRECTION('center_axis',(0.,-1.,0.));
#12716=DIRECTION('ref_axis',(1.,0.,0.));
#12717=DIRECTION('',(0.,-1.,0.));
#12718=DIRECTION('center_axis',(0.,-1.,0.));
#12719=DIRECTION('ref_axis',(1.,0.,0.));
#12720=DIRECTION('center_axis',(0.,1.,0.));
#12721=DIRECTION('ref_axis',(1.,0.,0.));
#12722=DIRECTION('center_axis',(0.,1.,0.));
#12723=DIRECTION('ref_axis',(1.,0.,0.));
#12724=DIRECTION('',(0.,-1.,0.));
#12725=DIRECTION('center_axis',(0.,1.,0.));
#12726=DIRECTION('ref_axis',(1.,0.,0.));
#12727=DIRECTION('center_axis',(0.,1.,0.));
#12728=DIRECTION('ref_axis',(1.,0.,0.));
#12729=DIRECTION('center_axis',(0.,1.,0.));
#12730=DIRECTION('ref_axis',(1.,0.,0.));
#12731=DIRECTION('axis',(0.,0.,1.));
#12732=DIRECTION('refdir',(1.,0.,0.));
#12733=DIRECTION('axis',(0.,0.,1.));
#12734=DIRECTION('refdir',(1.,0.,0.));
#12735=DIRECTION('center_axis',(0.,0.,1.));
#12736=DIRECTION('ref_axis',(1.,0.,0.));
#12737=DIRECTION('',(-1.,0.,0.));
#12738=DIRECTION('center_axis',(0.,0.,1.));
#12739=DIRECTION('ref_axis',(1.,0.,0.));
#12740=DIRECTION('center_axis',(0.,0.,1.));
#12741=DIRECTION('ref_axis',(1.,0.,0.));
#12742=DIRECTION('',(0.,0.,-1.));
#12743=DIRECTION('center_axis',(0.,0.,1.));
#12744=DIRECTION('ref_axis',(1.,0.,0.));
#12745=DIRECTION('',(0.,0.,1.));
#12746=DIRECTION('center_axis',(0.,0.,-1.));
#12747=DIRECTION('ref_axis',(1.,0.,0.));
#12748=DIRECTION('center_axis',(0.,0.,1.));
#12749=DIRECTION('ref_axis',(1.,0.,0.));
#12750=DIRECTION('',(0.,0.,1.));
#12751=DIRECTION('center_axis',(0.,0.,1.));
#12752=DIRECTION('ref_axis',(1.,0.,0.));
#12753=DIRECTION('',(1.,0.,0.));
#12754=DIRECTION('center_axis',(0.,0.,1.));
#12755=DIRECTION('ref_axis',(1.,0.,0.));
#12756=DIRECTION('center_axis',(0.,0.,1.));
#12757=DIRECTION('ref_axis',(1.,0.,0.));
#12758=DIRECTION('',(0.,0.,-1.));
#12759=DIRECTION('center_axis',(0.,0.,1.));
#12760=DIRECTION('ref_axis',(1.,0.,0.));
#12761=DIRECTION('',(0.,0.,1.));
#12762=DIRECTION('center_axis',(0.,0.,-1.));
#12763=DIRECTION('ref_axis',(1.,0.,0.));
#12764=DIRECTION('center_axis',(0.,0.,1.));
#12765=DIRECTION('ref_axis',(1.,0.,0.));
#12766=DIRECTION('',(0.,0.,1.));
#12767=DIRECTION('center_axis',(0.,0.,1.));
#12768=DIRECTION('ref_axis',(1.,0.,0.));
#12769=DIRECTION('',(-1.,0.,0.));
#12770=DIRECTION('center_axis',(0.,0.,1.));
#12771=DIRECTION('ref_axis',(1.,0.,0.));
#12772=DIRECTION('center_axis',(0.,0.,1.));
#12773=DIRECTION('ref_axis',(1.,0.,0.));
#12774=DIRECTION('',(0.,0.,-1.));
#12775=DIRECTION('center_axis',(0.,0.,1.));
#12776=DIRECTION('ref_axis',(1.,0.,0.));
#12777=DIRECTION('',(0.,0.,1.));
#12778=DIRECTION('center_axis',(0.,0.,-1.));
#12779=DIRECTION('ref_axis',(1.,0.,0.));
#12780=DIRECTION('center_axis',(0.,0.,1.));
#12781=DIRECTION('ref_axis',(1.,0.,0.));
#12782=DIRECTION('',(0.,0.,1.));
#12783=DIRECTION('center_axis',(0.,0.,1.));
#12784=DIRECTION('ref_axis',(1.,0.,0.));
#12785=DIRECTION('',(1.,0.,0.));
#12786=DIRECTION('center_axis',(0.,0.,1.));
#12787=DIRECTION('ref_axis',(1.,0.,0.));
#12788=DIRECTION('center_axis',(0.,0.,1.));
#12789=DIRECTION('ref_axis',(1.,0.,0.));
#12790=DIRECTION('',(0.,0.,-1.));
#12791=DIRECTION('center_axis',(0.,0.,1.));
#12792=DIRECTION('ref_axis',(1.,0.,0.));
#12793=DIRECTION('',(0.,0.,1.));
#12794=DIRECTION('center_axis',(0.,0.,-1.));
#12795=DIRECTION('ref_axis',(1.,0.,0.));
#12796=DIRECTION('center_axis',(0.,0.,1.));
#12797=DIRECTION('ref_axis',(1.,0.,0.));
#12798=DIRECTION('',(0.,0.,1.));
#12799=DIRECTION('center_axis',(0.,-1.,0.));
#12800=DIRECTION('ref_axis',(0.,0.,-1.));
#12801=DIRECTION('',(-1.,0.,0.));
#12802=DIRECTION('',(-1.,0.,0.));
#12803=DIRECTION('',(0.,0.,1.));
#12804=DIRECTION('',(1.,0.,0.));
#12805=DIRECTION('',(0.,0.,-1.));
#12806=DIRECTION('',(-1.,0.,0.));
#12807=DIRECTION('center_axis',(0.,1.,0.));
#12808=DIRECTION('ref_axis',(0.,0.,1.));
#12809=DIRECTION('',(1.,0.,0.));
#12810=DIRECTION('',(1.,0.,0.));
#12811=DIRECTION('',(0.,0.,1.));
#12812=DIRECTION('',(1.,0.,0.));
#12813=DIRECTION('',(0.,0.,-1.));
#12814=DIRECTION('',(1.,0.,0.));
#12815=DIRECTION('center_axis',(-1.,0.,0.));
#12816=DIRECTION('ref_axis',(0.,0.,1.));
#12817=DIRECTION('',(0.,-1.,0.));
#12818=DIRECTION('',(0.,0.,1.));
#12819=DIRECTION('',(0.,1.,0.));
#12820=DIRECTION('',(0.,0.,-1.));
#12821=DIRECTION('',(0.,-1.,0.));
#12822=DIRECTION('',(0.,-1.,0.));
#12823=DIRECTION('',(0.,0.,1.));
#12824=DIRECTION('',(0.,-1.,0.));
#12825=DIRECTION('',(0.,0.,-1.));
#12826=DIRECTION('',(0.,-1.,0.));
#12827=DIRECTION('center_axis',(0.,0.,-1.));
#12828=DIRECTION('ref_axis',(0.,1.,0.));
#12829=DIRECTION('',(0.,1.,0.));
#12830=DIRECTION('',(1.,0.,0.));
#12831=DIRECTION('center_axis',(0.,-1.,0.));
#12832=DIRECTION('ref_axis',(0.,0.,-1.));
#12833=DIRECTION('',(0.,0.,-1.));
#12834=DIRECTION('',(1.,0.,0.));
#12835=DIRECTION('center_axis',(0.,0.,1.));
#12836=DIRECTION('ref_axis',(0.,-1.,0.));
#12837=DIRECTION('',(0.,-1.,0.));
#12838=DIRECTION('',(1.,0.,0.));
#12839=DIRECTION('center_axis',(0.,1.,0.));
#12840=DIRECTION('ref_axis',(0.,0.,1.));
#12841=DIRECTION('',(0.,0.,1.));
#12842=DIRECTION('',(1.,0.,0.));
#12843=DIRECTION('center_axis',(0.,0.,-1.));
#12844=DIRECTION('ref_axis',(0.,1.,0.));
#12845=DIRECTION('',(0.,1.,0.));
#12846=DIRECTION('center_axis',(0.,0.,-1.));
#12847=DIRECTION('ref_axis',(0.,1.,0.));
#12848=DIRECTION('',(0.,1.,0.));
#12849=DIRECTION('',(1.,0.,0.));
#12850=DIRECTION('center_axis',(0.,-1.,0.));
#12851=DIRECTION('ref_axis',(0.,0.,-1.));
#12852=DIRECTION('',(0.,0.,-1.));
#12853=DIRECTION('',(1.,0.,0.));
#12854=DIRECTION('center_axis',(0.,0.,-1.));
#12855=DIRECTION('ref_axis',(0.,1.,0.));
#12856=DIRECTION('',(0.,1.,0.));
#12857=DIRECTION('',(1.,0.,0.));
#12858=DIRECTION('center_axis',(0.,1.,0.));
#12859=DIRECTION('ref_axis',(0.,0.,1.));
#12860=DIRECTION('',(0.,0.,1.));
#12861=DIRECTION('',(1.,0.,0.));
#12862=DIRECTION('center_axis',(0.,0.,-1.));
#12863=DIRECTION('ref_axis',(0.,1.,0.));
#12864=DIRECTION('',(0.,1.,0.));
#12865=DIRECTION('center_axis',(1.,0.,0.));
#12866=DIRECTION('ref_axis',(0.,0.,-1.));
#12867=DIRECTION('axis',(0.,0.,1.));
#12868=DIRECTION('refdir',(1.,0.,0.));
#12869=DIRECTION('center_axis',(0.,0.,1.));
#12870=DIRECTION('ref_axis',(0.,-1.,0.));
#12871=DIRECTION('',(0.,-1.,0.));
#12872=DIRECTION('',(1.,0.,0.));
#12873=DIRECTION('',(0.,-1.,0.));
#12874=DIRECTION('',(1.,0.,0.));
#12875=DIRECTION('center_axis',(0.,1.,0.));
#12876=DIRECTION('ref_axis',(0.,0.,1.));
#12877=DIRECTION('',(0.,0.,1.));
#12878=DIRECTION('',(0.,0.,1.));
#12879=DIRECTION('',(1.,0.,0.));
#12880=DIRECTION('center_axis',(0.,0.,-1.));
#12881=DIRECTION('ref_axis',(0.,1.,0.));
#12882=DIRECTION('',(0.,1.,0.));
#12883=DIRECTION('',(0.,1.,0.));
#12884=DIRECTION('',(1.,0.,0.));
#12885=DIRECTION('center_axis',(0.,-1.,0.));
#12886=DIRECTION('ref_axis',(0.,0.,-1.));
#12887=DIRECTION('',(0.,0.,-1.));
#12888=DIRECTION('',(0.,0.,-1.));
#12889=DIRECTION('',(1.,0.,0.));
#12890=DIRECTION('center_axis',(0.,0.,-1.));
#12891=DIRECTION('ref_axis',(0.,1.,0.));
#12892=DIRECTION('',(0.,1.,0.));
#12893=DIRECTION('',(0.,1.,0.));
#12894=DIRECTION('',(1.,0.,0.));
#12895=DIRECTION('center_axis',(0.,1.,0.));
#12896=DIRECTION('ref_axis',(0.,0.,1.));
#12897=DIRECTION('',(0.,0.,1.));
#12898=DIRECTION('',(0.,0.,1.));
#12899=DIRECTION('',(1.,0.,0.));
#12900=DIRECTION('center_axis',(0.,0.,-1.));
#12901=DIRECTION('ref_axis',(0.,1.,0.));
#12902=DIRECTION('',(0.,1.,0.));
#12903=DIRECTION('',(0.,1.,0.));
#12904=DIRECTION('',(1.,0.,0.));
#12905=DIRECTION('center_axis',(0.,-1.,0.));
#12906=DIRECTION('ref_axis',(0.,0.,-1.));
#12907=DIRECTION('',(0.,0.,-1.));
#12908=DIRECTION('',(0.,0.,-1.));
#12909=DIRECTION('center_axis',(1.,0.,0.));
#12910=DIRECTION('ref_axis',(0.,0.,-1.));
#12911=DIRECTION('center_axis',(1.,0.,0.));
#12912=DIRECTION('ref_axis',(0.,0.,-1.));
#12913=DIRECTION('axis',(0.,0.,1.));
#12914=DIRECTION('refdir',(1.,0.,0.));
#12915=DIRECTION('center_axis',(0.,0.,-1.));
#12916=DIRECTION('ref_axis',(0.,-1.,0.));
#12917=DIRECTION('',(0.,1.,0.));
#12918=DIRECTION('',(-1.,0.,0.));
#12919=DIRECTION('',(0.,-1.,0.));
#12920=DIRECTION('',(-1.,0.,0.));
#12921=DIRECTION('center_axis',(0.,1.,0.));
#12922=DIRECTION('ref_axis',(0.,0.,-1.));
#12923=DIRECTION('',(0.,0.,1.));
#12924=DIRECTION('',(0.,0.,-1.));
#12925=DIRECTION('',(-1.,0.,0.));
#12926=DIRECTION('center_axis',(0.,0.,-1.));
#12927=DIRECTION('ref_axis',(0.,-1.,0.));
#12928=DIRECTION('',(0.,1.,0.));
#12929=DIRECTION('',(0.,-1.,0.));
#12930=DIRECTION('',(-1.,0.,0.));
#12931=DIRECTION('center_axis',(0.,-1.,0.));
#12932=DIRECTION('ref_axis',(0.,0.,1.));
#12933=DIRECTION('',(0.,0.,-1.));
#12934=DIRECTION('',(0.,0.,1.));
#12935=DIRECTION('',(-1.,0.,0.));
#12936=DIRECTION('center_axis',(0.,0.,-1.));
#12937=DIRECTION('ref_axis',(0.,-1.,0.));
#12938=DIRECTION('',(0.,1.,0.));
#12939=DIRECTION('',(0.,-1.,0.));
#12940=DIRECTION('',(-1.,0.,0.));
#12941=DIRECTION('center_axis',(0.,1.,0.));
#12942=DIRECTION('ref_axis',(0.,0.,-1.));
#12943=DIRECTION('',(0.,0.,1.));
#12944=DIRECTION('',(0.,0.,-1.));
#12945=DIRECTION('',(-1.,0.,0.));
#12946=DIRECTION('center_axis',(0.,0.,1.));
#12947=DIRECTION('ref_axis',(0.,1.,0.));
#12948=DIRECTION('',(0.,-1.,0.));
#12949=DIRECTION('',(0.,1.,0.));
#12950=DIRECTION('',(-1.,0.,0.));
#12951=DIRECTION('center_axis',(0.,-1.,0.));
#12952=DIRECTION('ref_axis',(0.,0.,1.));
#12953=DIRECTION('',(0.,0.,-1.));
#12954=DIRECTION('',(0.,0.,1.));
#12955=DIRECTION('center_axis',(1.,0.,0.));
#12956=DIRECTION('ref_axis',(0.,0.,-1.));
#12957=DIRECTION('center_axis',(-1.,0.,0.));
#12958=DIRECTION('ref_axis',(0.,0.,1.));
#12959=DIRECTION('',(0.,0.,1.));
#12960=DIRECTION('',(1.,0.,0.));
#12961=DIRECTION('',(0.,0.,1.));
#12962=DIRECTION('',(1.,0.,0.));
#12963=DIRECTION('',(0.,0.,1.));
#12964=DIRECTION('',(1.,0.,0.));
#12965=DIRECTION('axis',(0.,0.,1.));
#12966=DIRECTION('refdir',(1.,0.,0.));
#12967=DIRECTION('center_axis',(0.866025403784439,0.,-0.5));
#12968=DIRECTION('ref_axis',(0.5,0.,0.866025403784439));
#12969=DIRECTION('',(-0.5,0.,-0.866025403784439));
#12970=DIRECTION('',(0.,-1.,0.));
#12971=DIRECTION('',(0.5,0.,0.866025403784439));
#12972=DIRECTION('',(0.,-1.,0.));
#12973=DIRECTION('center_axis',(1.20185167898973E-16,0.,-1.));
#12974=DIRECTION('ref_axis',(1.,0.,1.20185167898973E-16));
#12975=DIRECTION('',(-1.,0.,-1.20185167898973E-16));
#12976=DIRECTION('',(0.,-1.,0.));
#12977=DIRECTION('',(1.,0.,1.20185167898973E-16));
#12978=DIRECTION('center_axis',(-0.866025403784439,0.,-0.5));
#12979=DIRECTION('ref_axis',(0.5,0.,-0.866025403784439));
#12980=DIRECTION('',(-0.5,0.,0.866025403784439));
#12981=DIRECTION('',(0.,-1.,0.));
#12982=DIRECTION('',(0.5,0.,-0.866025403784439));
#12983=DIRECTION('center_axis',(-0.866025403784439,0.,0.5));
#12984=DIRECTION('ref_axis',(-0.5,0.,-0.866025403784439));
#12985=DIRECTION('',(0.5,0.,0.866025403784439));
#12986=DIRECTION('',(0.,-1.,0.));
#12987=DIRECTION('',(-0.5,0.,-0.866025403784439));
#12988=DIRECTION('center_axis',(-2.40370335797945E-16,0.,1.));
#12989=DIRECTION('ref_axis',(-1.,0.,-2.40370335797945E-16));
#12990=DIRECTION('',(1.,0.,2.40370335797945E-16));
#12991=DIRECTION('',(0.,-1.,0.));
#12992=DIRECTION('',(-1.,0.,-2.40370335797945E-16));
#12993=DIRECTION('center_axis',(0.866025403784439,0.,0.5));
#12994=DIRECTION('ref_axis',(-0.5,0.,0.866025403784439));
#12995=DIRECTION('',(0.5,0.,-0.866025403784439));
#12996=DIRECTION('',(-0.5,0.,0.866025403784439));
#12997=DIRECTION('center_axis',(0.,1.,0.));
#12998=DIRECTION('ref_axis',(1.,0.,0.));
#12999=DIRECTION('center_axis',(0.,-1.,0.));
#13000=DIRECTION('ref_axis',(0.,0.,-1.));
#13001=DIRECTION('center_axis',(0.,1.,0.));
#13002=DIRECTION('ref_axis',(1.,0.,0.));
#13003=DIRECTION('center_axis',(0.,1.,0.));
#13004=DIRECTION('ref_axis',(1.,0.,0.));
#13005=DIRECTION('center_axis',(0.,1.,0.));
#13006=DIRECTION('ref_axis',(0.,0.,1.));
#13007=DIRECTION('center_axis',(0.,-1.,0.));
#13008=DIRECTION('ref_axis',(1.,0.,0.));
#13009=DIRECTION('center_axis',(0.,-1.,0.));
#13010=DIRECTION('ref_axis',(1.,0.,0.));
#13011=DIRECTION('center_axis',(0.,-1.,0.));
#13012=DIRECTION('ref_axis',(1.,0.,0.));
#13013=DIRECTION('',(0.707106781186548,0.707106781186547,8.65956056235493E-17));
#13014=DIRECTION('center_axis',(0.,-1.,0.));
#13015=DIRECTION('ref_axis',(1.,0.,0.));
#13016=DIRECTION('center_axis',(0.,-1.,0.));
#13017=DIRECTION('ref_axis',(1.,0.,0.));
#13018=DIRECTION('',(0.,1.,0.));
#13019=DIRECTION('center_axis',(0.,1.,0.));
#13020=DIRECTION('ref_axis',(1.,0.,0.));
#13021=DIRECTION('center_axis',(0.,-1.,0.));
#13022=DIRECTION('ref_axis',(1.,0.,0.));
#13023=DIRECTION('',(-0.707106781186547,0.707106781186548,-8.65956056235493E-17));
#13024=DIRECTION('center_axis',(0.,-1.,0.));
#13025=DIRECTION('ref_axis',(0.,0.,-1.));
#13026=DIRECTION('center_axis',(0.,-1.,0.));
#13027=DIRECTION('ref_axis',(1.,0.,0.));
#13028=DIRECTION('center_axis',(0.,1.,0.));
#13029=DIRECTION('ref_axis',(1.,0.,0.));
#13030=DIRECTION('center_axis',(0.,1.,0.));
#13031=DIRECTION('ref_axis',(1.,0.,0.));
#13032=DIRECTION('',(-0.447213595499958,0.894427190999916,-5.47678698264203E-17));
#13033=DIRECTION('center_axis',(0.,-1.,0.));
#13034=DIRECTION('ref_axis',(1.,0.,0.));
#13035=DIRECTION('',(0.,1.,0.));
#13036=DIRECTION('axis',(0.,0.,1.));
#13037=DIRECTION('refdir',(1.,0.,0.));
#13038=DIRECTION('center_axis',(0.,1.,0.));
#13039=DIRECTION('ref_axis',(1.,0.,0.));
#13040=DIRECTION('center_axis',(0.,1.,0.));
#13041=DIRECTION('ref_axis',(1.,0.,0.));
#13042=DIRECTION('',(0.707106781186548,-0.707106781186547,-8.65956056235494E-17));
#13043=DIRECTION('center_axis',(0.,-1.,0.));
#13044=DIRECTION('ref_axis',(1.,0.,0.));
#13045=DIRECTION('center_axis',(0.,1.,0.));
#13046=DIRECTION('ref_axis',(1.,0.,0.));
#13047=DIRECTION('',(0.,-1.,0.));
#13048=DIRECTION('center_axis',(0.,-1.,0.));
#13049=DIRECTION('ref_axis',(1.,0.,0.));
#13050=DIRECTION('center_axis',(0.,1.,0.));
#13051=DIRECTION('ref_axis',(1.,0.,0.));
#13052=DIRECTION('center_axis',(0.,1.,0.));
#13053=DIRECTION('ref_axis',(1.,0.,0.));
#13054=DIRECTION('center_axis',(0.,1.,0.));
#13055=DIRECTION('ref_axis',(1.,0.,0.));
#13056=DIRECTION('',(0.,-1.,0.));
#13057=DIRECTION('center_axis',(0.,1.,0.));
#13058=DIRECTION('ref_axis',(1.,0.,0.));
#13059=DIRECTION('center_axis',(0.,1.,0.));
#13060=DIRECTION('ref_axis',(1.,0.,0.));
#13061=DIRECTION('axis',(0.,0.,1.));
#13062=DIRECTION('refdir',(1.,0.,0.));
#13063=DIRECTION('center_axis',(0.,1.,0.));
#13064=DIRECTION('ref_axis',(0.,0.,1.));
#13065=DIRECTION('center_axis',(0.,-1.,0.));
#13066=DIRECTION('ref_axis',(1.,0.,0.));
#13067=DIRECTION('center_axis',(0.,-1.,0.));
#13068=DIRECTION('ref_axis',(1.,0.,0.));
#13069=DIRECTION('center_axis',(0.,-1.,0.));
#13070=DIRECTION('ref_axis',(1.,0.,0.));
#13071=DIRECTION('',(0.707106781186548,0.707106781186547,8.65956056235493E-17));
#13072=DIRECTION('center_axis',(0.,-1.,0.));
#13073=DIRECTION('ref_axis',(1.,0.,0.));
#13074=DIRECTION('center_axis',(0.,-1.,0.));
#13075=DIRECTION('ref_axis',(1.,0.,0.));
#13076=DIRECTION('',(0.,1.,0.));
#13077=DIRECTION('center_axis',(0.,1.,0.));
#13078=DIRECTION('ref_axis',(1.,0.,0.));
#13079=DIRECTION('center_axis',(0.,-1.,0.));
#13080=DIRECTION('ref_axis',(1.,0.,0.));
#13081=DIRECTION('',(-0.707106781186547,0.707106781186548,-8.65956056235493E-17));
#13082=DIRECTION('center_axis',(0.,-1.,0.));
#13083=DIRECTION('ref_axis',(0.,0.,-1.));
#13084=DIRECTION('center_axis',(0.,-1.,0.));
#13085=DIRECTION('ref_axis',(1.,0.,0.));
#13086=DIRECTION('center_axis',(0.,1.,0.));
#13087=DIRECTION('ref_axis',(1.,0.,0.));
#13088=DIRECTION('center_axis',(0.,1.,0.));
#13089=DIRECTION('ref_axis',(1.,0.,0.));
#13090=DIRECTION('',(-0.447213595499958,0.894427190999916,-5.47678698264203E-17));
#13091=DIRECTION('center_axis',(0.,-1.,0.));
#13092=DIRECTION('ref_axis',(1.,0.,0.));
#13093=DIRECTION('center_axis',(0.,1.,0.));
#13094=DIRECTION('ref_axis',(1.,0.,0.));
#13095=DIRECTION('',(0.,1.,0.));
#13096=DIRECTION('center_axis',(0.,1.,0.));
#13097=DIRECTION('ref_axis',(1.,0.,0.));
#13098=DIRECTION('center_axis',(0.,-1.,0.));
#13099=DIRECTION('ref_axis',(1.,0.,0.));
#13100=DIRECTION('',(-0.707106781186547,0.707106781186548,-8.65956056235493E-17));
#13101=DIRECTION('center_axis',(0.,-1.,0.));
#13102=DIRECTION('ref_axis',(0.,0.,-1.));
#13103=DIRECTION('center_axis',(0.866025403784439,0.,-0.5));
#13104=DIRECTION('ref_axis',(0.5,0.,0.866025403784439));
#13105=DIRECTION('',(-0.5,0.,-0.866025403784439));
#13106=DIRECTION('',(0.,-1.,0.));
#13107=DIRECTION('',(0.5,0.,0.866025403784439));
#13108=DIRECTION('',(0.,-1.,0.));
#13109=DIRECTION('center_axis',(1.20185167898973E-16,0.,-1.));
#13110=DIRECTION('ref_axis',(1.,0.,1.20185167898973E-16));
#13111=DIRECTION('',(-1.,0.,-1.20185167898973E-16));
#13112=DIRECTION('',(0.,-1.,0.));
#13113=DIRECTION('',(1.,0.,1.20185167898973E-16));
#13114=DIRECTION('center_axis',(-0.866025403784439,0.,-0.5));
#13115=DIRECTION('ref_axis',(0.5,0.,-0.866025403784439));
#13116=DIRECTION('',(-0.5,0.,0.866025403784439));
#13117=DIRECTION('',(0.,-1.,0.));
#13118=DIRECTION('',(0.5,0.,-0.866025403784439));
#13119=DIRECTION('center_axis',(-0.866025403784439,0.,0.5));
#13120=DIRECTION('ref_axis',(-0.5,0.,-0.866025403784439));
#13121=DIRECTION('',(0.5,0.,0.866025403784439));
#13122=DIRECTION('',(0.,-1.,0.));
#13123=DIRECTION('',(-0.5,0.,-0.866025403784439));
#13124=DIRECTION('center_axis',(-2.40370335797945E-16,0.,1.));
#13125=DIRECTION('ref_axis',(-1.,0.,-2.40370335797945E-16));
#13126=DIRECTION('',(1.,0.,2.40370335797945E-16));
#13127=DIRECTION('',(0.,-1.,0.));
#13128=DIRECTION('',(-1.,0.,-2.40370335797945E-16));
#13129=DIRECTION('center_axis',(0.866025403784439,0.,0.5));
#13130=DIRECTION('ref_axis',(-0.5,0.,0.866025403784439));
#13131=DIRECTION('',(0.5,0.,-0.866025403784439));
#13132=DIRECTION('',(-0.5,0.,0.866025403784439));
#13133=DIRECTION('center_axis',(0.,1.,0.));
#13134=DIRECTION('ref_axis',(1.,0.,0.));
#13135=DIRECTION('center_axis',(0.,-1.,0.));
#13136=DIRECTION('ref_axis',(0.,0.,-1.));
#13137=DIRECTION('',(0.,0.,1.));
#13138=DIRECTION('',(1.,0.,0.));
#13139=DIRECTION('',(0.,0.,1.));
#13140=DIRECTION('',(1.,0.,0.));
#13141=DIRECTION('',(0.,0.,1.));
#13142=DIRECTION('',(1.,0.,0.));
#13143=DIRECTION('',(0.,0.,1.));
#13144=DIRECTION('',(1.,0.,0.));
#13145=DIRECTION('',(0.,0.,1.));
#13146=DIRECTION('',(1.,0.,0.));
#13147=DIRECTION('',(0.,0.,1.));
#13148=DIRECTION('',(1.,0.,0.));
#13149=DIRECTION('',(0.,0.,1.));
#13150=DIRECTION('',(1.,0.,0.));
#13151=DIRECTION('',(0.,0.,1.));
#13152=DIRECTION('',(1.,0.,0.));
#13153=DIRECTION('',(0.,0.,1.));
#13154=DIRECTION('',(1.,0.,0.));
#13155=DIRECTION('',(0.,0.,1.));
#13156=DIRECTION('',(1.,0.,0.));
#13157=DIRECTION('',(0.,-1.,2.22044604925031E-16));
#13158=DIRECTION('',(1.,0.,0.));
#13159=DIRECTION('',(0.,-1.,2.22044604925031E-16));
#13160=DIRECTION('',(1.,0.,0.));
#13161=DIRECTION('',(0.,-1.,2.22044604925031E-16));
#13162=DIRECTION('',(1.,0.,0.));
#13163=DIRECTION('',(0.,-1.,2.22044604925031E-16));
#13164=DIRECTION('',(1.,0.,0.));
#13165=DIRECTION('',(0.,0.,1.));
#13166=DIRECTION('',(1.,0.,0.));
#13167=DIRECTION('',(0.,-1.,2.22044604925031E-16));
#13168=DIRECTION('',(1.,0.,0.));
#13169=DIRECTION('',(0.,-1.,2.22044604925031E-16));
#13170=DIRECTION('',(1.,0.,0.));
#13171=DIRECTION('',(0.,-1.,2.22044604925031E-16));
#13172=DIRECTION('',(1.,0.,0.));
#13173=DIRECTION('',(0.,-1.,2.22044604925031E-16));
#13174=DIRECTION('',(1.,0.,0.));
#13175=DIRECTION('',(0.,-1.,2.22044604925031E-16));
#13176=DIRECTION('',(1.,0.,0.));
#13177=DIRECTION('',(0.,-1.,2.22044604925031E-16));
#13178=DIRECTION('',(1.,0.,0.));
#13179=DIRECTION('',(0.,-1.,2.22044604925031E-16));
#13180=DIRECTION('',(1.,0.,0.));
#13181=DIRECTION('',(0.,-1.,2.22044604925031E-16));
#13182=DIRECTION('',(1.,0.,0.));
#13183=DIRECTION('',(0.,0.,1.));
#13184=DIRECTION('',(1.,0.,0.));
#13185=DIRECTION('',(0.,-1.,2.22044604925031E-16));
#13186=DIRECTION('',(1.,0.,0.));
#13187=DIRECTION('',(0.,-1.,2.22044604925031E-16));
#13188=DIRECTION('',(1.,0.,0.));
#13189=DIRECTION('',(0.,-1.,2.22044604925031E-16));
#13190=DIRECTION('',(1.,0.,0.));
#13191=DIRECTION('',(0.,-1.,2.22044604925031E-16));
#13192=DIRECTION('',(1.,0.,0.));
#13193=DIRECTION('',(0.,-1.,2.22044604925031E-16));
#13194=DIRECTION('',(1.,0.,0.));
#13195=DIRECTION('',(0.,-1.,2.22044604925031E-16));
#13196=DIRECTION('',(1.,0.,0.));
#13197=DIRECTION('',(0.,-1.,2.22044604925031E-16));
#13198=DIRECTION('',(1.,0.,0.));
#13199=DIRECTION('',(0.,-1.,2.22044604925031E-16));
#13200=DIRECTION('',(1.,0.,0.));
#13201=DIRECTION('',(0.,0.,1.));
#13202=DIRECTION('',(1.,0.,0.));
#13203=DIRECTION('',(0.,-1.,2.22044604925031E-16));
#13204=DIRECTION('',(1.,0.,0.));
#13205=DIRECTION('',(0.,-1.,2.22044604925031E-16));
#13206=DIRECTION('',(1.,0.,0.));
#13207=DIRECTION('',(0.,-1.,2.22044604925031E-16));
#13208=DIRECTION('',(1.,0.,0.));
#13209=DIRECTION('',(0.,-1.,2.22044604925031E-16));
#13210=DIRECTION('',(1.,0.,0.));
#13211=DIRECTION('axis',(0.,0.,1.));
#13212=DIRECTION('refdir',(1.,0.,0.));
#13213=DIRECTION('center_axis',(0.866025403784439,0.,-0.5));
#13214=DIRECTION('ref_axis',(0.5,0.,0.866025403784439));
#13215=DIRECTION('',(-0.5,0.,-0.866025403784439));
#13216=DIRECTION('',(0.,-1.,0.));
#13217=DIRECTION('',(0.5,0.,0.866025403784439));
#13218=DIRECTION('',(0.,-1.,0.));
#13219=DIRECTION('center_axis',(1.60246890531964E-16,0.,-1.));
#13220=DIRECTION('ref_axis',(1.,0.,1.60246890531964E-16));
#13221=DIRECTION('',(-1.,0.,-1.60246890531964E-16));
#13222=DIRECTION('',(0.,-1.,0.));
#13223=DIRECTION('',(1.,0.,1.60246890531964E-16));
#13224=DIRECTION('center_axis',(-0.866025403784439,0.,-0.5));
#13225=DIRECTION('ref_axis',(0.5,0.,-0.866025403784439));
#13226=DIRECTION('',(-0.5,0.,0.866025403784439));
#13227=DIRECTION('',(0.,-1.,0.));
#13228=DIRECTION('',(0.5,0.,-0.866025403784439));
#13229=DIRECTION('center_axis',(-0.866025403784439,0.,0.5));
#13230=DIRECTION('ref_axis',(-0.5,0.,-0.866025403784439));
#13231=DIRECTION('',(0.5,0.,0.866025403784439));
#13232=DIRECTION('',(0.,-1.,0.));
#13233=DIRECTION('',(-0.5,0.,-0.866025403784439));
#13234=DIRECTION('center_axis',(-1.60246890531964E-16,0.,1.));
#13235=DIRECTION('ref_axis',(-1.,0.,-1.60246890531964E-16));
#13236=DIRECTION('',(1.,0.,1.60246890531964E-16));
#13237=DIRECTION('',(0.,-1.,0.));
#13238=DIRECTION('',(-1.,0.,-1.60246890531964E-16));
#13239=DIRECTION('center_axis',(0.866025403784439,0.,0.5));
#13240=DIRECTION('ref_axis',(-0.5,0.,0.866025403784439));
#13241=DIRECTION('',(0.5,0.,-0.866025403784439));
#13242=DIRECTION('',(-0.5,0.,0.866025403784439));
#13243=DIRECTION('center_axis',(0.,1.,0.));
#13244=DIRECTION('ref_axis',(1.,0.,0.));
#13245=DIRECTION('center_axis',(0.,-1.,0.));
#13246=DIRECTION('ref_axis',(0.,0.,-1.));
#13247=DIRECTION('center_axis',(0.,1.,0.));
#13248=DIRECTION('ref_axis',(1.,0.,0.));
#13249=DIRECTION('center_axis',(0.,1.,0.));
#13250=DIRECTION('ref_axis',(1.,0.,0.));
#13251=DIRECTION('center_axis',(0.,1.,0.));
#13252=DIRECTION('ref_axis',(0.,0.,1.));
#13253=DIRECTION('center_axis',(0.,-1.,0.));
#13254=DIRECTION('ref_axis',(1.,0.,0.));
#13255=DIRECTION('center_axis',(0.,-1.,0.));
#13256=DIRECTION('ref_axis',(1.,0.,0.));
#13257=DIRECTION('center_axis',(0.,-1.,0.));
#13258=DIRECTION('ref_axis',(1.,0.,0.));
#13259=DIRECTION('',(0.707106781186547,0.707106781186548,8.65956056235493E-17));
#13260=DIRECTION('center_axis',(0.,-1.,0.));
#13261=DIRECTION('ref_axis',(1.,0.,0.));
#13262=DIRECTION('center_axis',(0.,-1.,0.));
#13263=DIRECTION('ref_axis',(1.,0.,0.));
#13264=DIRECTION('',(0.,1.,0.));
#13265=DIRECTION('center_axis',(0.,1.,0.));
#13266=DIRECTION('ref_axis',(1.,0.,0.));
#13267=DIRECTION('center_axis',(0.,-1.,0.));
#13268=DIRECTION('ref_axis',(1.,0.,0.));
#13269=DIRECTION('',(-0.707106781186547,0.707106781186548,-8.65956056235493E-17));
#13270=DIRECTION('center_axis',(0.,-1.,0.));
#13271=DIRECTION('ref_axis',(0.,0.,-1.));
#13272=DIRECTION('center_axis',(0.,-1.,0.));
#13273=DIRECTION('ref_axis',(1.,0.,0.));
#13274=DIRECTION('center_axis',(0.,1.,0.));
#13275=DIRECTION('ref_axis',(1.,0.,0.));
#13276=DIRECTION('center_axis',(0.,1.,0.));
#13277=DIRECTION('ref_axis',(1.,0.,0.));
#13278=DIRECTION('',(-0.447213595499958,0.894427190999916,-5.47678698264203E-17));
#13279=DIRECTION('center_axis',(0.,-1.,0.));
#13280=DIRECTION('ref_axis',(1.,0.,0.));
#13281=DIRECTION('',(0.,1.,0.));
#13282=DIRECTION('',(0.,0.,1.));
#13283=DIRECTION('',(1.,0.,0.));
#13284=DIRECTION('',(0.,0.,1.));
#13285=DIRECTION('',(1.,0.,0.));
#13286=DIRECTION('',(0.,0.,1.));
#13287=DIRECTION('',(1.,0.,0.));
#13288=DIRECTION('',(0.,0.,1.));
#13289=DIRECTION('',(1.,0.,0.));
#13290=DIRECTION('',(0.,0.,1.));
#13291=DIRECTION('',(1.,0.,0.));
#13292=DIRECTION('',(0.,0.,1.));
#13293=DIRECTION('',(1.,0.,0.));
#13294=DIRECTION('',(0.,0.,1.));
#13295=DIRECTION('',(1.,0.,0.));
#13296=DIRECTION('',(0.,0.,1.));
#13297=DIRECTION('',(1.,0.,0.));
#13298=DIRECTION('',(0.,0.,1.));
#13299=DIRECTION('',(1.,0.,0.));
#13300=DIRECTION('',(8.65956056235493E-17,-8.65956056235493E-17,-1.));
#13301=DIRECTION('',(2.22044604925031E-16,1.,-8.65956056235494E-17));
#13302=DIRECTION('',(0.,-1.,2.22044604925031E-16));
#13303=DIRECTION('',(1.,0.,0.));
#13304=DIRECTION('',(0.,-1.,2.22044604925031E-16));
#13305=DIRECTION('',(1.,0.,0.));
#13306=DIRECTION('',(0.,-1.,2.22044604925031E-16));
#13307=DIRECTION('',(1.,0.,0.));
#13308=DIRECTION('',(0.,0.,1.));
#13309=DIRECTION('',(1.,0.,0.));
#13310=DIRECTION('',(0.,0.,1.));
#13311=DIRECTION('',(1.,0.,0.));
#13312=DIRECTION('',(0.,0.,1.));
#13313=DIRECTION('',(1.,0.,0.));
#13314=DIRECTION('',(0.,0.,1.));
#13315=DIRECTION('',(1.,0.,0.));
#13316=DIRECTION('',(0.,0.,1.));
#13317=DIRECTION('',(1.,0.,0.));
#13318=DIRECTION('',(0.,0.,1.));
#13319=DIRECTION('',(1.,0.,0.));
#13320=DIRECTION('',(0.,0.,1.));
#13321=DIRECTION('',(1.,0.,0.));
#13322=DIRECTION('',(0.,0.,1.));
#13323=DIRECTION('',(1.,0.,0.));
#13324=DIRECTION('',(0.,-1.,2.22044604925031E-16));
#13325=DIRECTION('',(1.,0.,0.));
#13326=DIRECTION('',(0.,-1.,2.22044604925031E-16));
#13327=DIRECTION('',(1.,0.,0.));
#13328=DIRECTION('',(0.,-1.,2.22044604925031E-16));
#13329=DIRECTION('',(1.,0.,0.));
#13330=DIRECTION('',(0.,-1.,2.22044604925031E-16));
#13331=DIRECTION('',(1.,0.,0.));
#13332=DIRECTION('',(0.,-1.,2.22044604925031E-16));
#13333=DIRECTION('',(1.,0.,0.));
#13334=DIRECTION('',(0.,-1.,2.22044604925031E-16));
#13335=DIRECTION('',(1.,0.,0.));
#13336=DIRECTION('',(0.,-1.,2.22044604925031E-16));
#13337=DIRECTION('',(1.,0.,0.));
#13338=DIRECTION('',(0.,-1.,2.22044604925031E-16));
#13339=DIRECTION('',(1.,0.,0.));
#13340=DIRECTION('',(0.,-1.,2.22044604925031E-16));
#13341=DIRECTION('',(1.,0.,0.));
#13342=DIRECTION('',(0.,-1.,2.22044604925031E-16));
#13343=DIRECTION('',(1.,0.,0.));
#13344=DIRECTION('',(0.,-1.,2.22044604925031E-16));
#13345=DIRECTION('',(1.,0.,0.));
#13346=DIRECTION('',(0.,-1.,2.22044604925031E-16));
#13347=DIRECTION('',(1.,0.,0.));
#13348=DIRECTION('',(0.,0.,1.));
#13349=DIRECTION('',(1.,0.,0.));
#13350=DIRECTION('',(0.,0.,1.));
#13351=DIRECTION('',(1.,0.,0.));
#13352=DIRECTION('',(0.,0.,1.));
#13353=DIRECTION('',(1.,0.,0.));
#13354=DIRECTION('',(0.,0.,1.));
#13355=DIRECTION('',(1.,0.,0.));
#13356=DIRECTION('',(0.,0.,1.));
#13357=DIRECTION('',(1.,0.,0.));
#13358=CARTESIAN_POINT('',(0.,0.,0.));
#13359=CARTESIAN_POINT('',(0.,0.,0.));
#13360=CARTESIAN_POINT('',(0.,0.,0.));
#13361=CARTESIAN_POINT('Origin',(23.,-2.4,-0.1));
#13362=CARTESIAN_POINT('',(22.79,-2.4,0.));
#13363=CARTESIAN_POINT('Origin',(23.,-2.4,0.));
#13364=CARTESIAN_POINT('',(22.79,-2.4,1.));
#13365=CARTESIAN_POINT('',(22.79,-2.4,-0.1));
#13366=CARTESIAN_POINT('Origin',(23.,-2.4,1.));
#13367=CARTESIAN_POINT('Origin',(3.,2.4,-0.1));
#13368=CARTESIAN_POINT('',(2.79,2.4,0.));
#13369=CARTESIAN_POINT('Origin',(3.,2.4,0.));
#13370=CARTESIAN_POINT('',(2.79,2.4,1.));
#13371=CARTESIAN_POINT('',(2.79,2.4,-0.1));
#13372=CARTESIAN_POINT('Origin',(3.,2.4,1.));
#13373=CARTESIAN_POINT('Origin',(3.,-2.4,-0.1));
#13374=CARTESIAN_POINT('',(2.79,-2.4,0.));
#13375=CARTESIAN_POINT('Origin',(3.,-2.4,0.));
#13376=CARTESIAN_POINT('',(2.79,-2.4,1.));
#13377=CARTESIAN_POINT('',(2.79,-2.4,-0.1));
#13378=CARTESIAN_POINT('Origin',(3.,-2.4,1.));
#13379=CARTESIAN_POINT('Origin',(23.,2.4,-0.1));
#13380=CARTESIAN_POINT('',(22.79,2.4,0.));
#13381=CARTESIAN_POINT('Origin',(23.,2.4,0.));
#13382=CARTESIAN_POINT('',(22.79,2.4,1.));
#13383=CARTESIAN_POINT('',(22.79,2.4,-0.1));
#13384=CARTESIAN_POINT('Origin',(23.,2.4,1.));
#13385=CARTESIAN_POINT('Origin',(5.8,-8.5,-0.1));
#13386=CARTESIAN_POINT('',(5.59,-8.5,0.));
#13387=CARTESIAN_POINT('Origin',(5.8,-8.5,0.));
#13388=CARTESIAN_POINT('',(5.59,-8.5,1.));
#13389=CARTESIAN_POINT('',(5.59,-8.5,-0.1));
#13390=CARTESIAN_POINT('Origin',(5.8,-8.5,1.));
#13391=CARTESIAN_POINT('Origin',(-5.8,-5.5,-0.1));
#13392=CARTESIAN_POINT('',(-6.01,-5.5,0.));
#13393=CARTESIAN_POINT('Origin',(-5.8,-5.5,0.));
#13394=CARTESIAN_POINT('',(-6.01,-5.5,1.));
#13395=CARTESIAN_POINT('',(-6.01,-5.5,-0.1));
#13396=CARTESIAN_POINT('Origin',(-5.8,-5.5,1.));
#13397=CARTESIAN_POINT('Origin',(-5.8,-8.5,-0.1));
#13398=CARTESIAN_POINT('',(-6.01,-8.5,0.));
#13399=CARTESIAN_POINT('Origin',(-5.8,-8.5,0.));
#13400=CARTESIAN_POINT('',(-6.01,-8.5,1.));
#13401=CARTESIAN_POINT('',(-6.01,-8.5,-0.1));
#13402=CARTESIAN_POINT('Origin',(-5.8,-8.5,1.));
#13403=CARTESIAN_POINT('Origin',(5.8,-5.5,-0.1));
#13404=CARTESIAN_POINT('',(5.59,-5.5,0.));
#13405=CARTESIAN_POINT('Origin',(5.8,-5.5,0.));
#13406=CARTESIAN_POINT('',(5.59,-5.5,1.));
#13407=CARTESIAN_POINT('',(5.59,-5.5,-0.1));
#13408=CARTESIAN_POINT('Origin',(5.8,-5.5,1.));
#13409=CARTESIAN_POINT('Origin',(5.8,-16.5,-0.1));
#13410=CARTESIAN_POINT('',(5.59,-16.5,0.));
#13411=CARTESIAN_POINT('Origin',(5.8,-16.5,0.));
#13412=CARTESIAN_POINT('',(5.59,-16.5,1.));
#13413=CARTESIAN_POINT('',(5.59,-16.5,-0.1));
#13414=CARTESIAN_POINT('Origin',(5.8,-16.5,1.));
#13415=CARTESIAN_POINT('Origin',(-5.8,-13.5,-0.1));
#13416=CARTESIAN_POINT('',(-6.01,-13.5,0.));
#13417=CARTESIAN_POINT('Origin',(-5.8,-13.5,0.));
#13418=CARTESIAN_POINT('',(-6.01,-13.5,1.));
#13419=CARTESIAN_POINT('',(-6.01,-13.5,-0.1));
#13420=CARTESIAN_POINT('Origin',(-5.8,-13.5,1.));
#13421=CARTESIAN_POINT('Origin',(-5.8,-16.5,-0.1));
#13422=CARTESIAN_POINT('',(-6.01,-16.5,0.));
#13423=CARTESIAN_POINT('Origin',(-5.8,-16.5,0.));
#13424=CARTESIAN_POINT('',(-6.01,-16.5,1.));
#13425=CARTESIAN_POINT('',(-6.01,-16.5,-0.1));
#13426=CARTESIAN_POINT('Origin',(-5.8,-16.5,1.));
#13427=CARTESIAN_POINT('Origin',(5.8,-13.5,-0.1));
#13428=CARTESIAN_POINT('',(5.59,-13.5,0.));
#13429=CARTESIAN_POINT('Origin',(5.8,-13.5,0.));
#13430=CARTESIAN_POINT('',(5.59,-13.5,1.));
#13431=CARTESIAN_POINT('',(5.59,-13.5,-0.1));
#13432=CARTESIAN_POINT('Origin',(5.8,-13.5,1.));
#13433=CARTESIAN_POINT('Origin',(24.,9.,0.));
#13434=CARTESIAN_POINT('',(24.,9.,0.));
#13435=CARTESIAN_POINT('',(-8.,9.,0.));
#13436=CARTESIAN_POINT('',(24.,9.,0.));
#13437=CARTESIAN_POINT('',(-8.,9.,1.));
#13438=CARTESIAN_POINT('',(-8.,9.,0.));
#13439=CARTESIAN_POINT('',(24.,9.,1.));
#13440=CARTESIAN_POINT('',(24.,9.,1.));
#13441=CARTESIAN_POINT('',(24.,9.,0.));
#13442=CARTESIAN_POINT('Origin',(24.,-18.,0.));
#13443=CARTESIAN_POINT('',(24.,-18.,0.));
#13444=CARTESIAN_POINT('',(24.,-18.,0.));
#13445=CARTESIAN_POINT('',(24.,-18.,1.));
#13446=CARTESIAN_POINT('',(24.,-18.,1.));
#13447=CARTESIAN_POINT('',(24.,-18.,0.));
#13448=CARTESIAN_POINT('Origin',(-8.,-18.,0.));
#13449=CARTESIAN_POINT('',(-8.,-18.,0.));
#13450=CARTESIAN_POINT('',(-8.,-18.,0.));
#13451=CARTESIAN_POINT('',(-8.,-18.,1.));
#13452=CARTESIAN_POINT('',(-8.,-18.,1.));
#13453=CARTESIAN_POINT('',(-8.,-18.,0.));
#13454=CARTESIAN_POINT('Origin',(-8.,9.,0.));
#13455=CARTESIAN_POINT('',(-8.,9.,0.));
#13456=CARTESIAN_POINT('',(-8.,9.,1.));
#13457=CARTESIAN_POINT('Origin',(8.,-4.5,1.));
#13458=CARTESIAN_POINT('Origin',(8.,-4.5,0.));
#13459=CARTESIAN_POINT('',(0.,0.,0.));
#13460=CARTESIAN_POINT('Origin',(-4.75,-15.,7.3));
#13461=CARTESIAN_POINT('',(-5.09,-15.,7.3));
#13462=CARTESIAN_POINT('Origin',(-4.75,-15.,7.3));
#13463=CARTESIAN_POINT('',(-5.09,-15.,8.67));
#13464=CARTESIAN_POINT('',(-5.09,-15.,7.3));
#13465=CARTESIAN_POINT('Origin',(-4.75,-15.,8.67));
#13466=CARTESIAN_POINT('Origin',(-4.75,-15.,7.3));
#13467=CARTESIAN_POINT('Origin',(4.75,-15.,7.3));
#13468=CARTESIAN_POINT('',(4.41,-15.,7.3));
#13469=CARTESIAN_POINT('Origin',(4.75,-15.,7.3));
#13470=CARTESIAN_POINT('',(4.41,-15.,8.67));
#13471=CARTESIAN_POINT('',(4.41,-15.,7.3));
#13472=CARTESIAN_POINT('Origin',(4.75,-15.,8.67));
#13473=CARTESIAN_POINT('Origin',(4.75,-15.,7.3));
#13474=CARTESIAN_POINT('Origin',(5.8,-16.5,2.2));
#13475=CARTESIAN_POINT('',(5.3,-16.5,2.2));
#13476=CARTESIAN_POINT('Origin',(5.8,-16.5,2.2));
#13477=CARTESIAN_POINT('',(5.3,-16.5,8.67));
#13478=CARTESIAN_POINT('',(5.3,-16.5,2.2));
#13479=CARTESIAN_POINT('Origin',(5.8,-16.5,8.67));
#13480=CARTESIAN_POINT('Origin',(5.8,-16.5,2.2));
#13481=CARTESIAN_POINT('',(5.525,-16.5,2.2));
#13482=CARTESIAN_POINT('Origin',(5.8,-16.5,2.2));
#13483=CARTESIAN_POINT('Origin',(-5.8,-13.5,2.2));
#13484=CARTESIAN_POINT('',(-6.3,-13.5,2.2));
#13485=CARTESIAN_POINT('Origin',(-5.8,-13.5,2.2));
#13486=CARTESIAN_POINT('',(-6.3,-13.5,8.67));
#13487=CARTESIAN_POINT('',(-6.3,-13.5,2.2));
#13488=CARTESIAN_POINT('Origin',(-5.8,-13.5,8.67));
#13489=CARTESIAN_POINT('Origin',(-5.8,-13.5,2.2));
#13490=CARTESIAN_POINT('',(-6.075,-13.5,2.2));
#13491=CARTESIAN_POINT('Origin',(-5.8,-13.5,2.2));
#13492=CARTESIAN_POINT('Origin',(-5.8,-16.5,2.2));
#13493=CARTESIAN_POINT('',(-6.3,-16.5,2.2));
#13494=CARTESIAN_POINT('Origin',(-5.8,-16.5,2.2));
#13495=CARTESIAN_POINT('',(-6.3,-16.5,8.67));
#13496=CARTESIAN_POINT('',(-6.3,-16.5,2.2));
#13497=CARTESIAN_POINT('Origin',(-5.8,-16.5,8.67));
#13498=CARTESIAN_POINT('Origin',(-5.8,-16.5,2.2));
#13499=CARTESIAN_POINT('',(-6.075,-16.5,2.2));
#13500=CARTESIAN_POINT('Origin',(-5.8,-16.5,2.2));
#13501=CARTESIAN_POINT('Origin',(5.8,-13.5,2.2));
#13502=CARTESIAN_POINT('',(5.3,-13.5,2.2));
#13503=CARTESIAN_POINT('Origin',(5.8,-13.5,2.2));
#13504=CARTESIAN_POINT('',(5.3,-13.5,8.67));
#13505=CARTESIAN_POINT('',(5.3,-13.5,2.2));
#13506=CARTESIAN_POINT('Origin',(5.8,-13.5,8.67));
#13507=CARTESIAN_POINT('Origin',(5.8,-13.5,2.2));
#13508=CARTESIAN_POINT('',(5.525,-13.5,2.2));
#13509=CARTESIAN_POINT('Origin',(5.8,-13.5,2.2));
#13510=CARTESIAN_POINT('Origin',(5.8,-16.5,0.9));
#13511=CARTESIAN_POINT('',(5.525,-16.5,1.));
#13512=CARTESIAN_POINT('Origin',(5.8,-16.5,1.));
#13513=CARTESIAN_POINT('',(5.525,-16.5,0.9));
#13514=CARTESIAN_POINT('Origin',(-5.8,-13.5,0.9));
#13515=CARTESIAN_POINT('',(-6.075,-13.5,1.));
#13516=CARTESIAN_POINT('Origin',(-5.8,-13.5,1.));
#13517=CARTESIAN_POINT('',(-6.075,-13.5,0.9));
#13518=CARTESIAN_POINT('Origin',(-5.8,-16.5,0.9));
#13519=CARTESIAN_POINT('',(-6.075,-16.5,1.));
#13520=CARTESIAN_POINT('Origin',(-5.8,-16.5,1.));
#13521=CARTESIAN_POINT('',(-6.075,-16.5,0.9));
#13522=CARTESIAN_POINT('Origin',(5.8,-13.5,0.9));
#13523=CARTESIAN_POINT('',(5.525,-13.5,1.));
#13524=CARTESIAN_POINT('Origin',(5.8,-13.5,1.));
#13525=CARTESIAN_POINT('',(5.525,-13.5,0.9));
#13526=CARTESIAN_POINT('Origin',(7.,-12.75,1.));
#13527=CARTESIAN_POINT('',(7.,-12.75,1.));
#13528=CARTESIAN_POINT('',(-7.,-12.75,1.));
#13529=CARTESIAN_POINT('',(7.,-12.75,1.));
#13530=CARTESIAN_POINT('',(-7.,-12.75,8.67));
#13531=CARTESIAN_POINT('',(-7.,-12.75,1.));
#13532=CARTESIAN_POINT('',(7.,-12.75,8.67));
#13533=CARTESIAN_POINT('',(7.,-12.75,8.67));
#13534=CARTESIAN_POINT('',(7.,-12.75,1.));
#13535=CARTESIAN_POINT('Origin',(7.,-17.25,1.));
#13536=CARTESIAN_POINT('',(7.,-17.25,1.));
#13537=CARTESIAN_POINT('',(7.,-17.25,1.));
#13538=CARTESIAN_POINT('',(7.,-17.25,8.67));
#13539=CARTESIAN_POINT('',(7.,-17.25,8.67));
#13540=CARTESIAN_POINT('',(7.,-17.25,1.));
#13541=CARTESIAN_POINT('Origin',(-7.,-17.25,1.));
#13542=CARTESIAN_POINT('',(-7.,-17.25,1.));
#13543=CARTESIAN_POINT('',(-7.,-17.25,1.));
#13544=CARTESIAN_POINT('',(-7.,-17.25,8.67));
#13545=CARTESIAN_POINT('',(-7.,-17.25,8.67));
#13546=CARTESIAN_POINT('',(-7.,-17.25,1.));
#13547=CARTESIAN_POINT('Origin',(-7.,-12.75,1.));
#13548=CARTESIAN_POINT('',(-7.,-12.75,1.));
#13549=CARTESIAN_POINT('',(-7.,-12.75,8.67));
#13550=CARTESIAN_POINT('Origin',(0.,-15.,8.67));
#13551=CARTESIAN_POINT('Origin',(0.,-15.,1.));
#13552=CARTESIAN_POINT('',(0.,0.,0.));
#13553=CARTESIAN_POINT('Origin',(-4.75,-15.,8.67));
#13554=CARTESIAN_POINT('',(-5.175,-15.,9.87));
#13555=CARTESIAN_POINT('Origin',(-4.75,-15.,9.87));
#13556=CARTESIAN_POINT('',(-5.175,-15.,8.67));
#13557=CARTESIAN_POINT('',(-5.175,-15.,8.67));
#13558=CARTESIAN_POINT('Origin',(-4.75,-15.,8.67));
#13559=CARTESIAN_POINT('Origin',(-4.75,-15.,8.67));
#13560=CARTESIAN_POINT('',(-5.395,-15.,9.87));
#13561=CARTESIAN_POINT('Origin',(-4.75,-15.,9.87));
#13562=CARTESIAN_POINT('',(-5.395,-15.,8.67));
#13563=CARTESIAN_POINT('',(-5.395,-15.,8.67));
#13564=CARTESIAN_POINT('Origin',(-4.75,-15.,8.67));
#13565=CARTESIAN_POINT('Origin',(-4.75,-15.,9.87));
#13566=CARTESIAN_POINT('Origin',(-4.75,-15.,8.67));
#13567=CARTESIAN_POINT('',(0.,0.,0.));
#13568=CARTESIAN_POINT('Origin',(4.75,-15.,8.67));
#13569=CARTESIAN_POINT('',(4.325,-15.,9.87));
#13570=CARTESIAN_POINT('Origin',(4.75,-15.,9.87));
#13571=CARTESIAN_POINT('',(4.325,-15.,8.67));
#13572=CARTESIAN_POINT('',(4.325,-15.,8.67));
#13573=CARTESIAN_POINT('Origin',(4.75,-15.,8.67));
#13574=CARTESIAN_POINT('Origin',(4.75,-15.,8.67));
#13575=CARTESIAN_POINT('',(4.105,-15.,9.87));
#13576=CARTESIAN_POINT('Origin',(4.75,-15.,9.87));
#13577=CARTESIAN_POINT('',(4.105,-15.,8.67));
#13578=CARTESIAN_POINT('',(4.105,-15.,8.67));
#13579=CARTESIAN_POINT('Origin',(4.75,-15.,8.67));
#13580=CARTESIAN_POINT('Origin',(4.75,-15.,9.87));
#13581=CARTESIAN_POINT('Origin',(4.75,-15.,8.67));
#13582=CARTESIAN_POINT('',(0.,0.,0.));
#13583=CARTESIAN_POINT('Origin',(-4.75,-7.,7.3));
#13584=CARTESIAN_POINT('',(-5.09,-7.,7.3));
#13585=CARTESIAN_POINT('Origin',(-4.75,-7.,7.3));
#13586=CARTESIAN_POINT('',(-5.09,-7.,8.67));
#13587=CARTESIAN_POINT('',(-5.09,-7.,7.3));
#13588=CARTESIAN_POINT('Origin',(-4.75,-7.,8.67));
#13589=CARTESIAN_POINT('Origin',(-4.75,-7.,7.3));
#13590=CARTESIAN_POINT('Origin',(4.75,-7.,7.3));
#13591=CARTESIAN_POINT('',(4.41,-7.,7.3));
#13592=CARTESIAN_POINT('Origin',(4.75,-7.,7.3));
#13593=CARTESIAN_POINT('',(4.41,-7.,8.67));
#13594=CARTESIAN_POINT('',(4.41,-7.,7.3));
#13595=CARTESIAN_POINT('Origin',(4.75,-7.,8.67));
#13596=CARTESIAN_POINT('Origin',(4.75,-7.,7.3));
#13597=CARTESIAN_POINT('Origin',(5.8,-8.5,2.2));
#13598=CARTESIAN_POINT('',(5.3,-8.5,2.2));
#13599=CARTESIAN_POINT('Origin',(5.8,-8.5,2.2));
#13600=CARTESIAN_POINT('',(5.3,-8.5,8.67));
#13601=CARTESIAN_POINT('',(5.3,-8.5,2.2));
#13602=CARTESIAN_POINT('Origin',(5.8,-8.5,8.67));
#13603=CARTESIAN_POINT('Origin',(5.8,-8.5,2.2));
#13604=CARTESIAN_POINT('',(5.525,-8.5,2.2));
#13605=CARTESIAN_POINT('Origin',(5.8,-8.5,2.2));
#13606=CARTESIAN_POINT('Origin',(-5.8,-5.5,2.2));
#13607=CARTESIAN_POINT('',(-6.3,-5.5,2.2));
#13608=CARTESIAN_POINT('Origin',(-5.8,-5.5,2.2));
#13609=CARTESIAN_POINT('',(-6.3,-5.5,8.67));
#13610=CARTESIAN_POINT('',(-6.3,-5.5,2.2));
#13611=CARTESIAN_POINT('Origin',(-5.8,-5.5,8.67));
#13612=CARTESIAN_POINT('Origin',(-5.8,-5.5,2.2));
#13613=CARTESIAN_POINT('',(-6.075,-5.5,2.2));
#13614=CARTESIAN_POINT('Origin',(-5.8,-5.5,2.2));
#13615=CARTESIAN_POINT('Origin',(-5.8,-8.5,2.2));
#13616=CARTESIAN_POINT('',(-6.3,-8.5,2.2));
#13617=CARTESIAN_POINT('Origin',(-5.8,-8.5,2.2));
#13618=CARTESIAN_POINT('',(-6.3,-8.5,8.67));
#13619=CARTESIAN_POINT('',(-6.3,-8.5,2.2));
#13620=CARTESIAN_POINT('Origin',(-5.8,-8.5,8.67));
#13621=CARTESIAN_POINT('Origin',(-5.8,-8.5,2.2));
#13622=CARTESIAN_POINT('',(-6.075,-8.5,2.2));
#13623=CARTESIAN_POINT('Origin',(-5.8,-8.5,2.2));
#13624=CARTESIAN_POINT('Origin',(5.8,-5.5,2.2));
#13625=CARTESIAN_POINT('',(5.3,-5.5,2.2));
#13626=CARTESIAN_POINT('Origin',(5.8,-5.5,2.2));
#13627=CARTESIAN_POINT('',(5.3,-5.5,8.67));
#13628=CARTESIAN_POINT('',(5.3,-5.5,2.2));
#13629=CARTESIAN_POINT('Origin',(5.8,-5.5,8.67));
#13630=CARTESIAN_POINT('Origin',(5.8,-5.5,2.2));
#13631=CARTESIAN_POINT('',(5.525,-5.5,2.2));
#13632=CARTESIAN_POINT('Origin',(5.8,-5.5,2.2));
#13633=CARTESIAN_POINT('Origin',(5.8,-8.5,0.9));
#13634=CARTESIAN_POINT('',(5.525,-8.5,1.));
#13635=CARTESIAN_POINT('Origin',(5.8,-8.5,1.));
#13636=CARTESIAN_POINT('',(5.525,-8.5,0.9));
#13637=CARTESIAN_POINT('Origin',(-5.8,-5.5,0.9));
#13638=CARTESIAN_POINT('',(-6.075,-5.5,1.));
#13639=CARTESIAN_POINT('Origin',(-5.8,-5.5,1.));
#13640=CARTESIAN_POINT('',(-6.075,-5.5,0.9));
#13641=CARTESIAN_POINT('Origin',(-5.8,-8.5,0.9));
#13642=CARTESIAN_POINT('',(-6.075,-8.5,1.));
#13643=CARTESIAN_POINT('Origin',(-5.8,-8.5,1.));
#13644=CARTESIAN_POINT('',(-6.075,-8.5,0.9));
#13645=CARTESIAN_POINT('Origin',(5.8,-5.5,0.9));
#13646=CARTESIAN_POINT('',(5.525,-5.5,1.));
#13647=CARTESIAN_POINT('Origin',(5.8,-5.5,1.));
#13648=CARTESIAN_POINT('',(5.525,-5.5,0.9));
#13649=CARTESIAN_POINT('Origin',(7.,-4.75,1.));
#13650=CARTESIAN_POINT('',(7.,-4.75,1.));
#13651=CARTESIAN_POINT('',(-7.,-4.75,1.));
#13652=CARTESIAN_POINT('',(7.,-4.75,1.));
#13653=CARTESIAN_POINT('',(-7.,-4.75,8.67));
#13654=CARTESIAN_POINT('',(-7.,-4.75,1.));
#13655=CARTESIAN_POINT('',(7.,-4.75,8.67));
#13656=CARTESIAN_POINT('',(7.,-4.75,8.67));
#13657=CARTESIAN_POINT('',(7.,-4.75,1.));
#13658=CARTESIAN_POINT('Origin',(7.,-9.25,1.));
#13659=CARTESIAN_POINT('',(7.,-9.25,1.));
#13660=CARTESIAN_POINT('',(7.,-9.25,1.));
#13661=CARTESIAN_POINT('',(7.,-9.25,8.67));
#13662=CARTESIAN_POINT('',(7.,-9.25,8.67));
#13663=CARTESIAN_POINT('',(7.,-9.25,1.));
#13664=CARTESIAN_POINT('Origin',(-7.,-9.25,1.));
#13665=CARTESIAN_POINT('',(-7.,-9.25,1.));
#13666=CARTESIAN_POINT('',(-7.,-9.25,1.));
#13667=CARTESIAN_POINT('',(-7.,-9.25,8.67));
#13668=CARTESIAN_POINT('',(-7.,-9.25,8.67));
#13669=CARTESIAN_POINT('',(-7.,-9.25,1.));
#13670=CARTESIAN_POINT('Origin',(-7.,-4.75,1.));
#13671=CARTESIAN_POINT('',(-7.,-4.75,1.));
#13672=CARTESIAN_POINT('',(-7.,-4.75,8.67));
#13673=CARTESIAN_POINT('Origin',(0.,-7.,8.67));
#13674=CARTESIAN_POINT('Origin',(0.,-7.,1.));
#13675=CARTESIAN_POINT('',(0.,0.,0.));
#13676=CARTESIAN_POINT('Origin',(-4.75,-7.,8.67));
#13677=CARTESIAN_POINT('',(-5.175,-7.,9.87));
#13678=CARTESIAN_POINT('Origin',(-4.75,-7.,9.87));
#13679=CARTESIAN_POINT('',(-5.175,-7.,8.67));
#13680=CARTESIAN_POINT('',(-5.175,-7.,8.67));
#13681=CARTESIAN_POINT('Origin',(-4.75,-7.,8.67));
#13682=CARTESIAN_POINT('Origin',(-4.75,-7.,8.67));
#13683=CARTESIAN_POINT('',(-5.395,-7.,9.87));
#13684=CARTESIAN_POINT('Origin',(-4.75,-7.,9.87));
#13685=CARTESIAN_POINT('',(-5.395,-7.,8.67));
#13686=CARTESIAN_POINT('',(-5.395,-7.,8.67));
#13687=CARTESIAN_POINT('Origin',(-4.75,-7.,8.67));
#13688=CARTESIAN_POINT('Origin',(-4.75,-7.,9.87));
#13689=CARTESIAN_POINT('Origin',(-4.75,-7.,8.67));
#13690=CARTESIAN_POINT('',(0.,0.,0.));
#13691=CARTESIAN_POINT('Origin',(4.75,-7.,8.67));
#13692=CARTESIAN_POINT('',(4.325,-7.,9.87));
#13693=CARTESIAN_POINT('Origin',(4.75,-7.,9.87));
#13694=CARTESIAN_POINT('',(4.325,-7.,8.67));
#13695=CARTESIAN_POINT('',(4.325,-7.,8.67));
#13696=CARTESIAN_POINT('Origin',(4.75,-7.,8.67));
#13697=CARTESIAN_POINT('Origin',(4.75,-7.,8.67));
#13698=CARTESIAN_POINT('',(4.105,-7.,9.87));
#13699=CARTESIAN_POINT('Origin',(4.75,-7.,9.87));
#13700=CARTESIAN_POINT('',(4.105,-7.,8.67));
#13701=CARTESIAN_POINT('',(4.105,-7.,8.67));
#13702=CARTESIAN_POINT('Origin',(4.75,-7.,8.67));
#13703=CARTESIAN_POINT('Origin',(4.75,-7.,9.87));
#13704=CARTESIAN_POINT('Origin',(4.75,-7.,8.67));
#13705=CARTESIAN_POINT('',(0.,0.,0.));
#13706=CARTESIAN_POINT('Origin',(16.,0.,3.5));
#13707=CARTESIAN_POINT('',(15.835,-2.02066721859312E-17,3.5));
#13708=CARTESIAN_POINT('Origin',(16.,0.,3.5));
#13709=CARTESIAN_POINT('',(15.835,2.02066721859312E-17,4.3));
#13710=CARTESIAN_POINT('',(15.835,-2.02066721859312E-17,3.5));
#13711=CARTESIAN_POINT('Origin',(16.,0.,4.3));
#13712=CARTESIAN_POINT('Origin',(16.,0.,3.5));
#13713=CARTESIAN_POINT('Origin',(10.,0.,3.5));
#13714=CARTESIAN_POINT('',(9.835,-2.02066721859312E-17,3.5));
#13715=CARTESIAN_POINT('Origin',(10.,0.,3.5));
#13716=CARTESIAN_POINT('',(9.835,2.02066721859312E-17,4.3));
#13717=CARTESIAN_POINT('',(9.835,-2.02066721859312E-17,3.5));
#13718=CARTESIAN_POINT('Origin',(10.,0.,4.3));
#13719=CARTESIAN_POINT('Origin',(10.,0.,3.5));
#13720=CARTESIAN_POINT('Origin',(4.,0.,3.5));
#13721=CARTESIAN_POINT('',(3.835,-2.02066721859313E-17,3.5));
#13722=CARTESIAN_POINT('Origin',(4.,0.,3.5));
#13723=CARTESIAN_POINT('',(3.835,2.02066721859313E-17,4.3));
#13724=CARTESIAN_POINT('',(3.835,-2.02066721859313E-17,3.5));
#13725=CARTESIAN_POINT('Origin',(4.,0.,4.3));
#13726=CARTESIAN_POINT('Origin',(4.,0.,3.5));
#13727=CARTESIAN_POINT('Origin',(22.,0.,3.5));
#13728=CARTESIAN_POINT('',(21.835,-2.02066721859312E-17,3.5));
#13729=CARTESIAN_POINT('Origin',(22.,0.,3.5));
#13730=CARTESIAN_POINT('',(21.835,2.02066721859312E-17,4.3));
#13731=CARTESIAN_POINT('',(21.835,-2.02066721859312E-17,3.5));
#13732=CARTESIAN_POINT('Origin',(22.,0.,4.3));
#13733=CARTESIAN_POINT('Origin',(22.,0.,3.5));
#13734=CARTESIAN_POINT('Origin',(23.,-2.4,2.2));
#13735=CARTESIAN_POINT('',(22.5,-2.4,2.2));
#13736=CARTESIAN_POINT('Origin',(23.,-2.4,2.2));
#13737=CARTESIAN_POINT('',(22.5,-2.4,4.3));
#13738=CARTESIAN_POINT('',(22.5,-2.4,2.2));
#13739=CARTESIAN_POINT('Origin',(23.,-2.4,4.3));
#13740=CARTESIAN_POINT('Origin',(23.,-2.4,2.2));
#13741=CARTESIAN_POINT('',(22.725,-2.4,2.2));
#13742=CARTESIAN_POINT('Origin',(23.,-2.4,2.2));
#13743=CARTESIAN_POINT('Origin',(3.,2.4,2.2));
#13744=CARTESIAN_POINT('',(2.5,2.4,2.2));
#13745=CARTESIAN_POINT('Origin',(3.,2.4,2.2));
#13746=CARTESIAN_POINT('',(2.5,2.4,4.3));
#13747=CARTESIAN_POINT('',(2.5,2.4,2.2));
#13748=CARTESIAN_POINT('Origin',(3.,2.4,4.3));
#13749=CARTESIAN_POINT('Origin',(3.,2.4,2.2));
#13750=CARTESIAN_POINT('',(2.725,2.4,2.2));
#13751=CARTESIAN_POINT('Origin',(3.,2.4,2.2));
#13752=CARTESIAN_POINT('Origin',(3.,-2.4,2.2));
#13753=CARTESIAN_POINT('',(2.5,-2.4,2.2));
#13754=CARTESIAN_POINT('Origin',(3.,-2.4,2.2));
#13755=CARTESIAN_POINT('',(2.5,-2.4,4.3));
#13756=CARTESIAN_POINT('',(2.5,-2.4,2.2));
#13757=CARTESIAN_POINT('Origin',(3.,-2.4,4.3));
#13758=CARTESIAN_POINT('Origin',(3.,-2.4,2.2));
#13759=CARTESIAN_POINT('',(2.725,-2.4,2.2));
#13760=CARTESIAN_POINT('Origin',(3.,-2.4,2.2));
#13761=CARTESIAN_POINT('Origin',(23.,2.4,2.2));
#13762=CARTESIAN_POINT('',(22.5,2.4,2.2));
#13763=CARTESIAN_POINT('Origin',(23.,2.4,2.2));
#13764=CARTESIAN_POINT('',(22.5,2.4,4.3));
#13765=CARTESIAN_POINT('',(22.5,2.4,2.2));
#13766=CARTESIAN_POINT('Origin',(23.,2.4,4.3));
#13767=CARTESIAN_POINT('Origin',(23.,2.4,2.2));
#13768=CARTESIAN_POINT('',(22.725,2.4,2.2));
#13769=CARTESIAN_POINT('Origin',(23.,2.4,2.2));
#13770=CARTESIAN_POINT('Origin',(23.,-2.4,0.9));
#13771=CARTESIAN_POINT('',(22.725,-2.4,1.));
#13772=CARTESIAN_POINT('Origin',(23.,-2.4,1.));
#13773=CARTESIAN_POINT('',(22.725,-2.4,0.9));
#13774=CARTESIAN_POINT('Origin',(3.,2.4,0.9));
#13775=CARTESIAN_POINT('',(2.725,2.4,1.));
#13776=CARTESIAN_POINT('Origin',(3.,2.4,1.));
#13777=CARTESIAN_POINT('',(2.725,2.4,0.9));
#13778=CARTESIAN_POINT('Origin',(3.,-2.4,0.9));
#13779=CARTESIAN_POINT('',(2.725,-2.4,1.));
#13780=CARTESIAN_POINT('Origin',(3.,-2.4,1.));
#13781=CARTESIAN_POINT('',(2.725,-2.4,0.9));
#13782=CARTESIAN_POINT('Origin',(23.,2.4,0.9));
#13783=CARTESIAN_POINT('',(22.725,2.4,1.));
#13784=CARTESIAN_POINT('Origin',(23.,2.4,1.));
#13785=CARTESIAN_POINT('',(22.725,2.4,0.9));
#13786=CARTESIAN_POINT('Origin',(24.,3.1,1.));
#13787=CARTESIAN_POINT('',(24.,3.1,1.));
#13788=CARTESIAN_POINT('',(2.,3.1,1.));
#13789=CARTESIAN_POINT('',(24.,3.1,1.));
#13790=CARTESIAN_POINT('',(2.,3.1,4.3));
#13791=CARTESIAN_POINT('',(2.,3.1,1.));
#13792=CARTESIAN_POINT('',(24.,3.1,4.3));
#13793=CARTESIAN_POINT('',(24.,3.1,4.3));
#13794=CARTESIAN_POINT('',(24.,3.1,1.));
#13795=CARTESIAN_POINT('Origin',(24.,-3.1,1.));
#13796=CARTESIAN_POINT('',(24.,-3.1,1.));
#13797=CARTESIAN_POINT('',(24.,-3.1,1.));
#13798=CARTESIAN_POINT('',(24.,-3.1,4.3));
#13799=CARTESIAN_POINT('',(24.,-3.1,4.3));
#13800=CARTESIAN_POINT('',(24.,-3.1,1.));
#13801=CARTESIAN_POINT('Origin',(2.,-3.1,1.));
#13802=CARTESIAN_POINT('',(2.,-3.1,1.));
#13803=CARTESIAN_POINT('',(2.,-3.1,1.));
#13804=CARTESIAN_POINT('',(2.,-3.1,4.3));
#13805=CARTESIAN_POINT('',(2.,-3.1,4.3));
#13806=CARTESIAN_POINT('',(2.,-3.1,1.));
#13807=CARTESIAN_POINT('Origin',(2.,3.1,1.));
#13808=CARTESIAN_POINT('',(2.,3.1,1.));
#13809=CARTESIAN_POINT('',(2.,3.1,4.3));
#13810=CARTESIAN_POINT('Origin',(13.,0.,4.3));
#13811=CARTESIAN_POINT('Origin',(13.,0.,1.));
#13812=CARTESIAN_POINT('',(0.,0.,0.));
#13813=CARTESIAN_POINT('Origin',(-6.,9.,-0.5));
#13814=CARTESIAN_POINT('',(-6.,9.,-0.5));
#13815=CARTESIAN_POINT('',(-8.,9.,-0.5));
#13816=CARTESIAN_POINT('',(-6.,9.,-0.5));
#13817=CARTESIAN_POINT('',(-8.,9.,0.));
#13818=CARTESIAN_POINT('',(-8.,9.,-0.5));
#13819=CARTESIAN_POINT('',(-6.,9.,0.));
#13820=CARTESIAN_POINT('',(-6.,9.,0.));
#13821=CARTESIAN_POINT('',(-6.,9.,-0.5));
#13822=CARTESIAN_POINT('Origin',(-6.,-18.,-0.5));
#13823=CARTESIAN_POINT('',(-6.,-18.,-0.5));
#13824=CARTESIAN_POINT('',(-6.,-18.,-0.5));
#13825=CARTESIAN_POINT('',(-6.,-18.,0.));
#13826=CARTESIAN_POINT('',(-6.,-18.,0.));
#13827=CARTESIAN_POINT('',(-6.,-18.,-0.5));
#13828=CARTESIAN_POINT('Origin',(-8.,-18.,-0.5));
#13829=CARTESIAN_POINT('',(-8.,-18.,-0.5));
#13830=CARTESIAN_POINT('',(-8.,-18.,-0.5));
#13831=CARTESIAN_POINT('',(-8.,-18.,0.));
#13832=CARTESIAN_POINT('',(-8.,-18.,0.));
#13833=CARTESIAN_POINT('',(-8.,-18.,-0.5));
#13834=CARTESIAN_POINT('Origin',(-8.,9.,-0.5));
#13835=CARTESIAN_POINT('',(-8.,9.,-0.5));
#13836=CARTESIAN_POINT('',(-8.,9.,0.));
#13837=CARTESIAN_POINT('Origin',(-7.,-4.5,0.));
#13838=CARTESIAN_POINT('Origin',(-7.,-4.5,-0.5));
#13839=CARTESIAN_POINT('',(0.,0.,0.));
#13840=CARTESIAN_POINT('Origin',(24.,9.,-0.5));
#13841=CARTESIAN_POINT('',(24.,9.,-0.5));
#13842=CARTESIAN_POINT('',(22.,9.,-0.5));
#13843=CARTESIAN_POINT('',(24.,9.,-0.5));
#13844=CARTESIAN_POINT('',(22.,9.,0.));
#13845=CARTESIAN_POINT('',(22.,9.,-0.5));
#13846=CARTESIAN_POINT('',(24.,9.,0.));
#13847=CARTESIAN_POINT('',(24.,9.,0.));
#13848=CARTESIAN_POINT('',(24.,9.,-0.5));
#13849=CARTESIAN_POINT('Origin',(24.,-18.,-0.5));
#13850=CARTESIAN_POINT('',(24.,-18.,-0.5));
#13851=CARTESIAN_POINT('',(24.,-18.,-0.5));
#13852=CARTESIAN_POINT('',(24.,-18.,0.));
#13853=CARTESIAN_POINT('',(24.,-18.,0.));
#13854=CARTESIAN_POINT('',(24.,-18.,-0.5));
#13855=CARTESIAN_POINT('Origin',(22.,-18.,-0.5));
#13856=CARTESIAN_POINT('',(22.,-18.,-0.5));
#13857=CARTESIAN_POINT('',(22.,-18.,-0.5));
#13858=CARTESIAN_POINT('',(22.,-18.,0.));
#13859=CARTESIAN_POINT('',(22.,-18.,0.));
#13860=CARTESIAN_POINT('',(22.,-18.,-0.5));
#13861=CARTESIAN_POINT('Origin',(22.,9.,-0.5));
#13862=CARTESIAN_POINT('',(22.,9.,-0.5));
#13863=CARTESIAN_POINT('',(22.,9.,0.));
#13864=CARTESIAN_POINT('Origin',(23.,-4.5,0.));
#13865=CARTESIAN_POINT('Origin',(23.,-4.5,-0.5));
#13866=CARTESIAN_POINT('',(0.,0.,0.));
#13867=CARTESIAN_POINT('',(0.,0.,0.));
#13868=CARTESIAN_POINT('Origin',(0.,0.,0.));
#13869=CARTESIAN_POINT('',(-2.05,-1.65,2.51052593825207E-16));
#13870=CARTESIAN_POINT('Origin',(0.,-1.65,0.));
#13871=CARTESIAN_POINT('',(-2.05,-1.14891252930761,-2.51052593825207E-16));
#13872=CARTESIAN_POINT('',(-2.05,0.,2.51052593825207E-16));
#13873=CARTESIAN_POINT('Origin',(0.,-1.14891252930761,0.));
#13874=CARTESIAN_POINT('Origin',(0.,0.,0.));
#13875=CARTESIAN_POINT('',(-2.05,1.14891252930761,2.51052593825207E-16));
#13876=CARTESIAN_POINT('Origin',(0.,1.14891252930761,0.));
#13877=CARTESIAN_POINT('',(-2.05,1.65,-2.51052593825207E-16));
#13878=CARTESIAN_POINT('',(-2.05,0.,2.51052593825207E-16));
#13879=CARTESIAN_POINT('Origin',(0.,1.65,0.));
#13880=CARTESIAN_POINT('Origin',(0.,0.,0.));
#13881=CARTESIAN_POINT('',(-1.43895998899814E-16,-1.76221774462768E-32,
-2.35));
#13882=CARTESIAN_POINT('',(-1.43895998899814E-16,-1.76221774462768E-32,
2.35));
#13883=CARTESIAN_POINT('Origin',(0.,0.,0.));
#13884=CARTESIAN_POINT('Origin',(0.,1.55,-1.49));
#13885=CARTESIAN_POINT('',(-3.76384615384615,1.55,-2.13));
#13886=CARTESIAN_POINT('',(-1.81744325908679,1.55,-2.13));
#13887=CARTESIAN_POINT('',(0.,1.55,-2.13));
#13888=CARTESIAN_POINT('',(-2.46585583768694,1.55,-1.32648218523477));
#13889=CARTESIAN_POINT('',(-1.68,1.55,-0.84));
#13890=CARTESIAN_POINT('Origin',(0.,1.55,0.));
#13891=CARTESIAN_POINT('Origin',(0.,1.55,-1.49));
#13892=CARTESIAN_POINT('',(1.81744325908679,1.55,-2.13));
#13893=CARTESIAN_POINT('',(3.76384615384615,1.55,-2.13));
#13894=CARTESIAN_POINT('',(0.,1.55,-2.13));
#13895=CARTESIAN_POINT('',(2.46585583768694,1.55,-1.32648218523477));
#13896=CARTESIAN_POINT('Origin',(0.,1.55,0.));
#13897=CARTESIAN_POINT('',(3.78,1.55,-2.14));
#13898=CARTESIAN_POINT('Origin',(0.,-1.55,-1.49));
#13899=CARTESIAN_POINT('',(-1.81744325908679,-1.55,-2.13));
#13900=CARTESIAN_POINT('',(-3.76384615384615,-1.55,-2.13));
#13901=CARTESIAN_POINT('',(0.,-1.55,-2.13));
#13902=CARTESIAN_POINT('',(-2.46585583768694,-1.55,-1.32648218523477));
#13903=CARTESIAN_POINT('Origin',(0.,-1.55,0.));
#13904=CARTESIAN_POINT('',(-1.68,-1.55,-0.84));
#13905=CARTESIAN_POINT('Origin',(-3.78,0.,-2.14));
#13906=CARTESIAN_POINT('',(-3.76384615384615,0.,-2.13));
#13907=CARTESIAN_POINT('',(-2.46585583768694,0.,-1.32648218523477));
#13908=CARTESIAN_POINT('Origin',(0.,-1.55,-1.49));
#13909=CARTESIAN_POINT('',(3.76384615384615,-1.55,-2.13));
#13910=CARTESIAN_POINT('',(1.81744325908679,-1.55,-2.13));
#13911=CARTESIAN_POINT('',(0.,-1.55,-2.13));
#13912=CARTESIAN_POINT('',(2.46585583768694,-1.55,-1.32648218523477));
#13913=CARTESIAN_POINT('',(3.78,-1.55,-2.14));
#13914=CARTESIAN_POINT('Origin',(0.,-1.55,0.));
#13915=CARTESIAN_POINT('Origin',(1.68,0.,-0.84));
#13916=CARTESIAN_POINT('',(3.76384615384615,0.,-2.13));
#13917=CARTESIAN_POINT('',(2.46585583768694,0.,-1.32648218523477));
#13918=CARTESIAN_POINT('Origin',(0.,0.,-2.13));
#13919=CARTESIAN_POINT('',(-6.35,1.9,-2.13));
#13920=CARTESIAN_POINT('',(-6.35,-1.9,-2.13));
#13921=CARTESIAN_POINT('',(-6.35,1.9,-2.13));
#13922=CARTESIAN_POINT('',(6.35,-1.9,-2.13));
#13923=CARTESIAN_POINT('',(-6.35,-1.9,-2.13));
#13924=CARTESIAN_POINT('',(6.35,1.9,-2.13));
#13925=CARTESIAN_POINT('',(6.35,-1.9,-2.13));
#13926=CARTESIAN_POINT('',(6.35,1.9,-2.13));
#13927=CARTESIAN_POINT('',(4.1,7.9602041944578E-17,-2.13));
#13928=CARTESIAN_POINT('Origin',(4.75,0.,-2.13));
#13929=CARTESIAN_POINT('',(-5.4,7.9602041944578E-17,-2.13));
#13930=CARTESIAN_POINT('Origin',(-4.75,0.,-2.13));
#13931=CARTESIAN_POINT('',(1.81744325908679,-1.65,-2.13));
#13932=CARTESIAN_POINT('',(1.81744325908679,0.,-2.13));
#13933=CARTESIAN_POINT('',(-1.81744325908679,-1.65,-2.13));
#13934=CARTESIAN_POINT('',(0.,-1.65,-2.13));
#13935=CARTESIAN_POINT('',(-1.81744325908679,0.,-2.13));
#13936=CARTESIAN_POINT('',(-1.81744325908679,1.65,-2.13));
#13937=CARTESIAN_POINT('',(-1.81744325908679,0.,-2.13));
#13938=CARTESIAN_POINT('',(1.81744325908679,1.65,-2.13));
#13939=CARTESIAN_POINT('',(0.,1.65,-2.13));
#13940=CARTESIAN_POINT('',(1.81744325908679,0.,-2.13));
#13941=CARTESIAN_POINT('Origin',(0.,0.,0.));
#13942=CARTESIAN_POINT('Origin',(0.,1.65,0.));
#13943=CARTESIAN_POINT('Origin',(0.,-1.65,0.));
#13944=CARTESIAN_POINT('Origin',(0.,-1.65,0.));
#13945=CARTESIAN_POINT('Origin',(0.,1.65,0.));
#13946=CARTESIAN_POINT('Origin',(3.35,1.4,-3.33));
#13947=CARTESIAN_POINT('',(3.35,1.4,-3.33));
#13948=CARTESIAN_POINT('',(-3.35,1.4,-3.33));
#13949=CARTESIAN_POINT('',(1.675,1.4,-3.33));
#13950=CARTESIAN_POINT('',(3.35,1.4,-2.83));
#13951=CARTESIAN_POINT('',(3.35,1.4,-3.33));
#13952=CARTESIAN_POINT('',(-3.35,1.4,-2.83));
#13953=CARTESIAN_POINT('',(3.35,1.4,-2.83));
#13954=CARTESIAN_POINT('',(-3.35,1.4,-3.33));
#13955=CARTESIAN_POINT('Origin',(3.35,-1.4,-3.33));
#13956=CARTESIAN_POINT('',(3.35,-1.4,-3.33));
#13957=CARTESIAN_POINT('',(3.35,-0.7,-3.33));
#13958=CARTESIAN_POINT('',(3.35,-1.4,-2.83));
#13959=CARTESIAN_POINT('',(3.35,-1.4,-3.33));
#13960=CARTESIAN_POINT('',(3.35,-1.4,-2.83));
#13961=CARTESIAN_POINT('Origin',(-3.35,-1.4,-3.33));
#13962=CARTESIAN_POINT('',(-3.35,-1.4,-3.33));
#13963=CARTESIAN_POINT('',(-1.675,-1.4,-3.33));
#13964=CARTESIAN_POINT('',(-3.35,-1.4,-2.83));
#13965=CARTESIAN_POINT('',(-3.35,-1.4,-3.33));
#13966=CARTESIAN_POINT('',(-3.35,-1.4,-2.83));
#13967=CARTESIAN_POINT('Origin',(-3.35,1.4,-3.33));
#13968=CARTESIAN_POINT('',(-3.35,0.7,-3.33));
#13969=CARTESIAN_POINT('',(-3.35,1.4,-2.83));
#13970=CARTESIAN_POINT('Origin',(0.,0.,-2.83));
#13971=CARTESIAN_POINT('Origin',(-4.75,0.,-3.33));
#13972=CARTESIAN_POINT('',(-5.4,-7.9602041944578E-17,-3.33));
#13973=CARTESIAN_POINT('Origin',(-4.75,0.,-3.33));
#13974=CARTESIAN_POINT('',(-5.4,-7.9602041944578E-17,-3.33));
#13975=CARTESIAN_POINT('Origin',(4.75,0.,-3.33));
#13976=CARTESIAN_POINT('',(4.1,-7.9602041944578E-17,-3.33));
#13977=CARTESIAN_POINT('Origin',(4.75,0.,-3.33));
#13978=CARTESIAN_POINT('',(4.1,-7.9602041944578E-17,-3.33));
#13979=CARTESIAN_POINT('Origin',(6.35,1.9,-3.33));
#13980=CARTESIAN_POINT('',(6.35,1.9,-3.33));
#13981=CARTESIAN_POINT('',(-6.35,1.9,-3.33));
#13982=CARTESIAN_POINT('',(6.35,1.9,-3.33));
#13983=CARTESIAN_POINT('',(-6.35,1.9,-3.33));
#13984=CARTESIAN_POINT('',(6.35,1.9,-3.33));
#13985=CARTESIAN_POINT('Origin',(6.35,-1.9,-3.33));
#13986=CARTESIAN_POINT('',(6.35,-1.9,-3.33));
#13987=CARTESIAN_POINT('',(6.35,-1.9,-3.33));
#13988=CARTESIAN_POINT('',(6.35,-1.9,-3.33));
#13989=CARTESIAN_POINT('Origin',(-6.35,-1.9,-3.33));
#13990=CARTESIAN_POINT('',(-6.35,-1.9,-3.33));
#13991=CARTESIAN_POINT('',(-6.35,-1.9,-3.33));
#13992=CARTESIAN_POINT('',(-6.35,-1.9,-3.33));
#13993=CARTESIAN_POINT('Origin',(-6.35,1.9,-3.33));
#13994=CARTESIAN_POINT('',(-6.35,1.9,-3.33));
#13995=CARTESIAN_POINT('Origin',(0.,0.,-3.33));
#13996=CARTESIAN_POINT('',(0.,0.,0.));
#13997=CARTESIAN_POINT('Origin',(0.,0.,0.));
#13998=CARTESIAN_POINT('',(-1.8,-0.85,-2.20436423846524E-16));
#13999=CARTESIAN_POINT('Origin',(0.,-0.85,0.));
#14000=CARTESIAN_POINT('',(-1.8,0.85,-2.20436423846524E-16));
#14001=CARTESIAN_POINT('',(-1.8,0.,-2.20436423846524E-16));
#14002=CARTESIAN_POINT('Origin',(0.,0.85,0.));
#14003=CARTESIAN_POINT('Origin',(2.19089023002066,0.85,0.));
#14004=CARTESIAN_POINT('',(2.19089023002066,0.85,0.));
#14005=CARTESIAN_POINT('Origin',(0.,0.85,0.));
#14006=CARTESIAN_POINT('Origin',(3.99680288865056E-15,0.,0.));
#14007=CARTESIAN_POINT('',(3.85290688975075E-15,-1.76221774462768E-32,2.35));
#14008=CARTESIAN_POINT('',(3.85290688975075E-15,-1.76221774462768E-32,-2.35));
#14009=CARTESIAN_POINT('Origin',(3.99680288865056E-15,0.,0.));
#14010=CARTESIAN_POINT('',(2.19089023002066,-0.85,0.));
#14011=CARTESIAN_POINT('Origin',(0.,-0.85,0.));
#14012=CARTESIAN_POINT('Origin',(1.8,-0.85,0.));
#14013=CARTESIAN_POINT('Origin',(0.,1.55,0.));
#14014=CARTESIAN_POINT('',(1.42894191624432,1.8,0.825000000000001));
#14015=CARTESIAN_POINT('',(1.53744468918255,1.55,0.598968970568896));
#14016=CARTESIAN_POINT('Ctrl Pts',(1.42894191624432,1.8,0.825000000000001));
#14017=CARTESIAN_POINT('Ctrl Pts',(1.44466308895875,1.8,0.797770130104052));
#14018=CARTESIAN_POINT('Ctrl Pts',(1.46055812562105,1.79370633789704,0.768258557763732));
#14019=CARTESIAN_POINT('Ctrl Pts',(1.48824888379079,1.76817777258318,0.713138492740816));
#14020=CARTESIAN_POINT('Ctrl Pts',(1.50008999307766,1.74894552961493,0.687551581002689));
#14021=CARTESIAN_POINT('Ctrl Pts',(1.51812136280714,1.70460745840382,0.646764802471699));
#14022=CARTESIAN_POINT('Ctrl Pts',(1.52552758004446,1.67652816181843,0.628833667319578));
#14023=CARTESIAN_POINT('Ctrl Pts',(1.53516661651472,1.61494799959182,0.604921184808251));
#14024=CARTESIAN_POINT('Ctrl Pts',(1.53744468918255,1.58144291640553,0.598968970568896));
#14025=CARTESIAN_POINT('Ctrl Pts',(1.53744468918255,1.55,0.598968970568896));
#14026=CARTESIAN_POINT('',(1.42894191624432,1.3,0.825000000000001));
#14027=CARTESIAN_POINT('Ctrl Pts',(1.42894191624432,1.3,0.825000000000001));
#14028=CARTESIAN_POINT('Ctrl Pts',(1.4132207435299,1.3,0.852229869895949));
#14029=CARTESIAN_POINT('Ctrl Pts',(1.39561049050871,1.30629366210296,0.880751161609749));
#14030=CARTESIAN_POINT('Ctrl Pts',(1.36172049302549,1.33182222741682,0.932292094146256));
#14031=CARTESIAN_POINT('Ctrl Pts',(1.34548213209931,1.35105447038507,0.955340251466734));
#14032=CARTESIAN_POINT('Ctrl Pts',(1.31917543061769,1.39539254159618,0.99134926498299));
#14033=CARTESIAN_POINT('Ctrl Pts',(1.30734972067592,1.42347183818157,1.00672880483252));
#14034=CARTESIAN_POINT('Ctrl Pts',(1.29146042158868,1.48505200040818,1.02703269653942));
#14035=CARTESIAN_POINT('Ctrl Pts',(1.28744468918255,1.51855708359447,1.03198167246111));
#14036=CARTESIAN_POINT('Ctrl Pts',(1.28744468918255,1.58144291640553,1.03198167246111));
#14037=CARTESIAN_POINT('Ctrl Pts',(1.29146042158868,1.61494799959182,1.02703269653942));
#14038=CARTESIAN_POINT('Ctrl Pts',(1.30734972067592,1.67652816181843,1.00672880483252));
#14039=CARTESIAN_POINT('Ctrl Pts',(1.31917543061769,1.70460745840382,0.991349264982991));
#14040=CARTESIAN_POINT('Ctrl Pts',(1.34548213209931,1.74894552961493,0.955340251466735));
#14041=CARTESIAN_POINT('Ctrl Pts',(1.36172049302549,1.76817777258318,0.932292094146256));
#14042=CARTESIAN_POINT('Ctrl Pts',(1.39561049050871,1.79370633789704,0.880751161609749));
#14043=CARTESIAN_POINT('Ctrl Pts',(1.4132207435299,1.8,0.85222986989595));
#14044=CARTESIAN_POINT('Ctrl Pts',(1.42894191624432,1.8,0.825000000000001));
#14045=CARTESIAN_POINT('Ctrl Pts',(1.53744468918255,1.55,0.598968970568896));
#14046=CARTESIAN_POINT('Ctrl Pts',(1.53744468918255,1.51855708359447,0.598968970568896));
#14047=CARTESIAN_POINT('Ctrl Pts',(1.53516661651472,1.48505200040818,0.60492118480825));
#14048=CARTESIAN_POINT('Ctrl Pts',(1.52552758004446,1.42347183818157,0.628833667319578));
#14049=CARTESIAN_POINT('Ctrl Pts',(1.51812136280714,1.39539254159618,0.646764802471699));
#14050=CARTESIAN_POINT('Ctrl Pts',(1.50008999307766,1.35105447038507,0.687551581002689));
#14051=CARTESIAN_POINT('Ctrl Pts',(1.48824888379079,1.33182222741682,0.713138492740816));
#14052=CARTESIAN_POINT('Ctrl Pts',(1.46055812562105,1.30629366210296,0.768258557763732));
#14053=CARTESIAN_POINT('Ctrl Pts',(1.44466308895875,1.3,0.797770130104052));
#14054=CARTESIAN_POINT('Ctrl Pts',(1.42894191624432,1.3,0.825000000000001));
#14055=CARTESIAN_POINT('',(0.963525491562421,1.55,0.267616567329818));
#14056=CARTESIAN_POINT('',(0.125,1.55,-0.21650635094611));
#14057=CARTESIAN_POINT('Ctrl Pts',(0.963525491562421,1.55,0.267616567329818));
#14058=CARTESIAN_POINT('Ctrl Pts',(0.963525491562421,1.5815373526696,0.267616567329818));
#14059=CARTESIAN_POINT('Ctrl Pts',(0.961833761492987,1.61508042700263,0.273949373987484));
#14060=CARTESIAN_POINT('Ctrl Pts',(0.954308486908894,1.67663267125761,0.299111603474268));
#14061=CARTESIAN_POINT('Ctrl Pts',(0.948394987258249,1.70465411363682,0.31788699900678));
#14062=CARTESIAN_POINT('Ctrl Pts',(0.933155485613026,1.74889618382539,0.360174810895352));
#14063=CARTESIAN_POINT('Ctrl Pts',(0.92278792026947,1.76811531482682,0.386546956384144));
#14064=CARTESIAN_POINT('Ctrl Pts',(0.897143218189782,1.79367084275751,0.442820664919227));
#14065=CARTESIAN_POINT('Ctrl Pts',(0.881791875377343,1.8,0.472691670144998));
#14066=CARTESIAN_POINT('Ctrl Pts',(0.850258932191534,1.8,0.527308329855003));
#14067=CARTESIAN_POINT('Ctrl Pts',(0.832065554235658,1.79367084275751,0.555538485325664));
#14068=CARTESIAN_POINT('Ctrl Pts',(0.796153444118959,1.76811531482682,0.605884303066698));
#14069=CARTESIAN_POINT('Ctrl Pts',(0.778498278845144,1.74889618382539,0.62804895077401));
#14070=CARTESIAN_POINT('Ctrl Pts',(0.749495710301794,1.70465411363682,0.662390652284073));
#14071=CARTESIAN_POINT('Ctrl Pts',(0.73619249062986,1.67663267125761,0.676899590973058));
#14072=CARTESIAN_POINT('Ctrl Pts',(0.718163997970498,1.61508042700263,0.695997784676728));
#14073=CARTESIAN_POINT('Ctrl Pts',(0.713525491562421,1.5815373526696,0.700629269222037));
#14074=CARTESIAN_POINT('Ctrl Pts',(0.713525491562421,1.5184626473304,0.700629269222037));
#14075=CARTESIAN_POINT('Ctrl Pts',(0.718163997970498,1.48491957299737,0.695997784676728));
#14076=CARTESIAN_POINT('Ctrl Pts',(0.73619249062986,1.42336732874239,0.676899590973058));
#14077=CARTESIAN_POINT('Ctrl Pts',(0.749495710301794,1.39534588636318,0.662390652284073));
#14078=CARTESIAN_POINT('Ctrl Pts',(0.778498278845144,1.35110381617461,0.62804895077401));
#14079=CARTESIAN_POINT('Ctrl Pts',(0.796153444118959,1.33188468517318,0.605884303066698));
#14080=CARTESIAN_POINT('Ctrl Pts',(0.832065554235658,1.30632915724249,0.555538485325664));
#14081=CARTESIAN_POINT('Ctrl Pts',(0.850258932191534,1.3,0.527308329855003));
#14082=CARTESIAN_POINT('Ctrl Pts',(0.881791875377343,1.3,0.472691670144998));
#14083=CARTESIAN_POINT('Ctrl Pts',(0.897143218189782,1.30632915724249,0.442820664919227));
#14084=CARTESIAN_POINT('Ctrl Pts',(0.92278792026947,1.33188468517318,0.386546956384144));
#14085=CARTESIAN_POINT('Ctrl Pts',(0.933155485613026,1.35110381617461,0.360174810895352));
#14086=CARTESIAN_POINT('Ctrl Pts',(0.948394987258249,1.39534588636318,0.31788699900678));
#14087=CARTESIAN_POINT('Ctrl Pts',(0.954308486908894,1.42336732874239,0.299111603474268));
#14088=CARTESIAN_POINT('Ctrl Pts',(0.961833761492987,1.48491957299738,0.273949373987484));
#14089=CARTESIAN_POINT('Ctrl Pts',(0.963525491562421,1.5184626473304,0.267616567329818));
#14090=CARTESIAN_POINT('Ctrl Pts',(0.963525491562421,1.55,0.267616567329818));
#14091=CARTESIAN_POINT('Origin',(0.,1.55,0.));
#14092=CARTESIAN_POINT('',(-0.713525491562421,1.55,-0.700629269222037));
#14093=CARTESIAN_POINT('Ctrl Pts',(-0.713525491562421,1.55,-0.700629269222037));
#14094=CARTESIAN_POINT('Ctrl Pts',(-0.713525491562421,1.5184626473304,-0.700629269222037));
#14095=CARTESIAN_POINT('Ctrl Pts',(-0.718163997970498,1.48491957299737,
-0.695997784676728));
#14096=CARTESIAN_POINT('Ctrl Pts',(-0.73619249062986,1.42336732874239,-0.676899590973058));
#14097=CARTESIAN_POINT('Ctrl Pts',(-0.749495710301794,1.39534588636318,
-0.662390652284073));
#14098=CARTESIAN_POINT('Ctrl Pts',(-0.778498278845144,1.35110381617461,
-0.62804895077401));
#14099=CARTESIAN_POINT('Ctrl Pts',(-0.796153444118959,1.33188468517318,
-0.605884303066698));
#14100=CARTESIAN_POINT('Ctrl Pts',(-0.832065554235658,1.30632915724249,
-0.555538485325664));
#14101=CARTESIAN_POINT('Ctrl Pts',(-0.850258932191534,1.3,-0.527308329855003));
#14102=CARTESIAN_POINT('Ctrl Pts',(-0.881791875377343,1.3,-0.472691670144998));
#14103=CARTESIAN_POINT('Ctrl Pts',(-0.897143218189782,1.30632915724249,
-0.442820664919227));
#14104=CARTESIAN_POINT('Ctrl Pts',(-0.92278792026947,1.33188468517318,-0.386546956384144));
#14105=CARTESIAN_POINT('Ctrl Pts',(-0.933155485613026,1.35110381617461,
-0.360174810895352));
#14106=CARTESIAN_POINT('Ctrl Pts',(-0.948394987258249,1.39534588636318,
-0.31788699900678));
#14107=CARTESIAN_POINT('Ctrl Pts',(-0.954308486908894,1.42336732874239,
-0.299111603474268));
#14108=CARTESIAN_POINT('Ctrl Pts',(-0.961833761492986,1.48491957299737,
-0.273949373987484));
#14109=CARTESIAN_POINT('Ctrl Pts',(-0.963525491562421,1.5184626473304,-0.267616567329818));
#14110=CARTESIAN_POINT('Ctrl Pts',(-0.963525491562421,1.5815373526696,-0.267616567329818));
#14111=CARTESIAN_POINT('Ctrl Pts',(-0.961833761492986,1.61508042700263,
-0.273949373987484));
#14112=CARTESIAN_POINT('Ctrl Pts',(-0.954308486908894,1.67663267125761,
-0.299111603474268));
#14113=CARTESIAN_POINT('Ctrl Pts',(-0.948394987258249,1.70465411363682,
-0.31788699900678));
#14114=CARTESIAN_POINT('Ctrl Pts',(-0.933155485613026,1.74889618382539,
-0.360174810895352));
#14115=CARTESIAN_POINT('Ctrl Pts',(-0.92278792026947,1.76811531482682,-0.386546956384144));
#14116=CARTESIAN_POINT('Ctrl Pts',(-0.897143218189782,1.79367084275751,
-0.442820664919227));
#14117=CARTESIAN_POINT('Ctrl Pts',(-0.881791875377343,1.8,-0.472691670144998));
#14118=CARTESIAN_POINT('Ctrl Pts',(-0.850258932191534,1.8,-0.527308329855003));
#14119=CARTESIAN_POINT('Ctrl Pts',(-0.832065554235658,1.79367084275751,
-0.555538485325664));
#14120=CARTESIAN_POINT('Ctrl Pts',(-0.796153444118959,1.76811531482682,
-0.605884303066698));
#14121=CARTESIAN_POINT('Ctrl Pts',(-0.778498278845144,1.74889618382539,
-0.62804895077401));
#14122=CARTESIAN_POINT('Ctrl Pts',(-0.749495710301794,1.70465411363682,
-0.662390652284073));
#14123=CARTESIAN_POINT('Ctrl Pts',(-0.73619249062986,1.67663267125761,-0.676899590973058));
#14124=CARTESIAN_POINT('Ctrl Pts',(-0.718163997970498,1.61508042700263,
-0.695997784676728));
#14125=CARTESIAN_POINT('Ctrl Pts',(-0.713525491562421,1.5815373526696,-0.700629269222037));
#14126=CARTESIAN_POINT('Ctrl Pts',(-0.713525491562421,1.55,-0.700629269222037));
#14127=CARTESIAN_POINT('',(-1.28744468918255,1.55,-1.03198167246111));
#14128=CARTESIAN_POINT('',(0.125,1.55,-0.21650635094611));
#14129=CARTESIAN_POINT('',(-1.42894191624432,1.3,-0.825000000000001));
#14130=CARTESIAN_POINT('Ctrl Pts',(-1.42894191624432,1.3,-0.825000000000001));
#14131=CARTESIAN_POINT('Ctrl Pts',(-1.4132207435299,1.3,-0.852229869895949));
#14132=CARTESIAN_POINT('Ctrl Pts',(-1.39561049050871,1.30629366210296,-0.880751161609749));
#14133=CARTESIAN_POINT('Ctrl Pts',(-1.36172049302549,1.33182222741682,-0.932292094146256));
#14134=CARTESIAN_POINT('Ctrl Pts',(-1.34548213209931,1.35105447038507,-0.955340251466735));
#14135=CARTESIAN_POINT('Ctrl Pts',(-1.31917543061769,1.39539254159618,-0.991349264982991));
#14136=CARTESIAN_POINT('Ctrl Pts',(-1.30734972067592,1.42347183818157,-1.00672880483252));
#14137=CARTESIAN_POINT('Ctrl Pts',(-1.29146042158868,1.48505200040818,-1.02703269653942));
#14138=CARTESIAN_POINT('Ctrl Pts',(-1.28744468918255,1.51855708359447,-1.03198167246111));
#14139=CARTESIAN_POINT('Ctrl Pts',(-1.28744468918255,1.55,-1.03198167246111));
#14140=CARTESIAN_POINT('',(-1.42894191624432,1.8,-0.825000000000001));
#14141=CARTESIAN_POINT('Ctrl Pts',(-1.42894191624432,1.8,-0.825000000000001));
#14142=CARTESIAN_POINT('Ctrl Pts',(-1.44466308895875,1.8,-0.797770130104052));
#14143=CARTESIAN_POINT('Ctrl Pts',(-1.46055812562105,1.79370633789704,-0.768258557763732));
#14144=CARTESIAN_POINT('Ctrl Pts',(-1.48824888379079,1.76817777258318,-0.713138492740816));
#14145=CARTESIAN_POINT('Ctrl Pts',(-1.50008999307766,1.74894552961493,-0.687551581002689));
#14146=CARTESIAN_POINT('Ctrl Pts',(-1.51812136280714,1.70460745840382,-0.646764802471699));
#14147=CARTESIAN_POINT('Ctrl Pts',(-1.52552758004446,1.67652816181843,-0.628833667319578));
#14148=CARTESIAN_POINT('Ctrl Pts',(-1.53516661651472,1.61494799959182,-0.60492118480825));
#14149=CARTESIAN_POINT('Ctrl Pts',(-1.53744468918255,1.58144291640553,-0.598968970568896));
#14150=CARTESIAN_POINT('Ctrl Pts',(-1.53744468918255,1.51855708359447,-0.598968970568896));
#14151=CARTESIAN_POINT('Ctrl Pts',(-1.53516661651472,1.48505200040818,-0.60492118480825));
#14152=CARTESIAN_POINT('Ctrl Pts',(-1.52552758004446,1.42347183818157,-0.628833667319578));
#14153=CARTESIAN_POINT('Ctrl Pts',(-1.51812136280714,1.39539254159618,-0.646764802471699));
#14154=CARTESIAN_POINT('Ctrl Pts',(-1.50008999307766,1.35105447038507,-0.687551581002689));
#14155=CARTESIAN_POINT('Ctrl Pts',(-1.48824888379079,1.33182222741682,-0.713138492740816));
#14156=CARTESIAN_POINT('Ctrl Pts',(-1.46055812562105,1.30629366210296,-0.768258557763732));
#14157=CARTESIAN_POINT('Ctrl Pts',(-1.44466308895875,1.3,-0.797770130104052));
#14158=CARTESIAN_POINT('Ctrl Pts',(-1.42894191624432,1.3,-0.825000000000001));
#14159=CARTESIAN_POINT('Ctrl Pts',(-1.28744468918255,1.55,-1.03198167246111));
#14160=CARTESIAN_POINT('Ctrl Pts',(-1.28744468918255,1.58144291640553,-1.03198167246111));
#14161=CARTESIAN_POINT('Ctrl Pts',(-1.29146042158868,1.61494799959182,-1.02703269653942));
#14162=CARTESIAN_POINT('Ctrl Pts',(-1.30734972067592,1.67652816181843,-1.00672880483252));
#14163=CARTESIAN_POINT('Ctrl Pts',(-1.31917543061769,1.70460745840382,-0.991349264982991));
#14164=CARTESIAN_POINT('Ctrl Pts',(-1.34548213209931,1.74894552961493,-0.955340251466734));
#14165=CARTESIAN_POINT('Ctrl Pts',(-1.36172049302549,1.76817777258318,-0.932292094146256));
#14166=CARTESIAN_POINT('Ctrl Pts',(-1.39561049050871,1.79370633789704,-0.880751161609749));
#14167=CARTESIAN_POINT('Ctrl Pts',(-1.4132207435299,1.8,-0.852229869895949));
#14168=CARTESIAN_POINT('Ctrl Pts',(-1.42894191624432,1.8,-0.825000000000001));
#14169=CARTESIAN_POINT('Origin',(0.,1.55,0.));
#14170=CARTESIAN_POINT('',(-1.65,0.85,-2.02066721859313E-16));
#14171=CARTESIAN_POINT('Origin',(0.,0.85,0.));
#14172=CARTESIAN_POINT('',(-1.65,2.25,-2.02066721859313E-16));
#14173=CARTESIAN_POINT('',(-1.65,1.55,-2.02066721859313E-16));
#14174=CARTESIAN_POINT('Origin',(0.,2.25,0.));
#14175=CARTESIAN_POINT('',(-1.42894191624432,1.3,0.825));
#14176=CARTESIAN_POINT('',(-1.42894191624432,1.8,0.825));
#14177=CARTESIAN_POINT('Ctrl Pts',(-1.42894191624432,1.3,0.825));
#14178=CARTESIAN_POINT('Ctrl Pts',(-1.44466308895875,1.3,0.797770130104051));
#14179=CARTESIAN_POINT('Ctrl Pts',(-1.46055812562105,1.30629366210296,0.768258557763731));
#14180=CARTESIAN_POINT('Ctrl Pts',(-1.48824888379079,1.33182222741682,0.713138492740815));
#14181=CARTESIAN_POINT('Ctrl Pts',(-1.50008999307766,1.35105447038507,0.687551581002688));
#14182=CARTESIAN_POINT('Ctrl Pts',(-1.51812136280714,1.39539254159618,0.646764802471698));
#14183=CARTESIAN_POINT('Ctrl Pts',(-1.52552758004446,1.42347183818157,0.628833667319577));
#14184=CARTESIAN_POINT('Ctrl Pts',(-1.53516661651472,1.48505200040818,0.604921184808249));
#14185=CARTESIAN_POINT('Ctrl Pts',(-1.53744468918255,1.51855708359447,0.598968970568895));
#14186=CARTESIAN_POINT('Ctrl Pts',(-1.53744468918255,1.58144291640553,0.598968970568895));
#14187=CARTESIAN_POINT('Ctrl Pts',(-1.53516661651472,1.61494799959182,0.604921184808249));
#14188=CARTESIAN_POINT('Ctrl Pts',(-1.52552758004446,1.67652816181843,0.628833667319577));
#14189=CARTESIAN_POINT('Ctrl Pts',(-1.51812136280714,1.70460745840382,0.646764802471698));
#14190=CARTESIAN_POINT('Ctrl Pts',(-1.50008999307766,1.74894552961493,0.687551581002688));
#14191=CARTESIAN_POINT('Ctrl Pts',(-1.48824888379079,1.76817777258318,0.713138492740815));
#14192=CARTESIAN_POINT('Ctrl Pts',(-1.46055812562105,1.79370633789704,0.768258557763731));
#14193=CARTESIAN_POINT('Ctrl Pts',(-1.44466308895875,1.8,0.797770130104051));
#14194=CARTESIAN_POINT('Ctrl Pts',(-1.42894191624432,1.8,0.825));
#14195=CARTESIAN_POINT('',(-1.28744468918255,1.55,1.03198167246111));
#14196=CARTESIAN_POINT('Ctrl Pts',(-1.42894191624432,1.8,0.825));
#14197=CARTESIAN_POINT('Ctrl Pts',(-1.4132207435299,1.8,0.852229869895948));
#14198=CARTESIAN_POINT('Ctrl Pts',(-1.39561049050871,1.79370633789704,0.880751161609747));
#14199=CARTESIAN_POINT('Ctrl Pts',(-1.36172049302549,1.76817777258318,0.932292094146255));
#14200=CARTESIAN_POINT('Ctrl Pts',(-1.34548213209931,1.74894552961493,0.955340251466733));
#14201=CARTESIAN_POINT('Ctrl Pts',(-1.31917543061769,1.70460745840382,0.991349264982989));
#14202=CARTESIAN_POINT('Ctrl Pts',(-1.30734972067592,1.67652816181843,1.00672880483252));
#14203=CARTESIAN_POINT('Ctrl Pts',(-1.29146042158868,1.61494799959182,1.02703269653942));
#14204=CARTESIAN_POINT('Ctrl Pts',(-1.28744468918255,1.58144291640553,1.03198167246111));
#14205=CARTESIAN_POINT('Ctrl Pts',(-1.28744468918255,1.55,1.03198167246111));
#14206=CARTESIAN_POINT('Ctrl Pts',(-1.28744468918255,1.55,1.03198167246111));
#14207=CARTESIAN_POINT('Ctrl Pts',(-1.28744468918255,1.51855708359447,1.03198167246111));
#14208=CARTESIAN_POINT('Ctrl Pts',(-1.29146042158868,1.48505200040818,1.02703269653942));
#14209=CARTESIAN_POINT('Ctrl Pts',(-1.30734972067592,1.42347183818157,1.00672880483252));
#14210=CARTESIAN_POINT('Ctrl Pts',(-1.31917543061769,1.39539254159618,0.99134926498299));
#14211=CARTESIAN_POINT('Ctrl Pts',(-1.34548213209931,1.35105447038508,0.955340251466733));
#14212=CARTESIAN_POINT('Ctrl Pts',(-1.36172049302549,1.33182222741682,0.932292094146255));
#14213=CARTESIAN_POINT('Ctrl Pts',(-1.39561049050871,1.30629366210296,0.880751161609748));
#14214=CARTESIAN_POINT('Ctrl Pts',(-1.4132207435299,1.3,0.852229869895949));
#14215=CARTESIAN_POINT('Ctrl Pts',(-1.42894191624432,1.3,0.825));
#14216=CARTESIAN_POINT('',(1.42894191624432,1.8,-0.825));
#14217=CARTESIAN_POINT('',(1.42894191624432,1.3,-0.825));
#14218=CARTESIAN_POINT('Ctrl Pts',(1.42894191624432,1.8,-0.825));
#14219=CARTESIAN_POINT('Ctrl Pts',(1.4132207435299,1.8,-0.852229869895949));
#14220=CARTESIAN_POINT('Ctrl Pts',(1.39561049050871,1.79370633789704,-0.880751161609748));
#14221=CARTESIAN_POINT('Ctrl Pts',(1.36172049302549,1.76817777258318,-0.932292094146255));
#14222=CARTESIAN_POINT('Ctrl Pts',(1.34548213209931,1.74894552961493,-0.955340251466734));
#14223=CARTESIAN_POINT('Ctrl Pts',(1.31917543061769,1.70460745840382,-0.99134926498299));
#14224=CARTESIAN_POINT('Ctrl Pts',(1.30734972067592,1.67652816181843,-1.00672880483252));
#14225=CARTESIAN_POINT('Ctrl Pts',(1.29146042158868,1.61494799959182,-1.02703269653942));
#14226=CARTESIAN_POINT('Ctrl Pts',(1.28744468918255,1.58144291640553,-1.03198167246111));
#14227=CARTESIAN_POINT('Ctrl Pts',(1.28744468918255,1.51855708359447,-1.03198167246111));
#14228=CARTESIAN_POINT('Ctrl Pts',(1.29146042158868,1.48505200040818,-1.02703269653942));
#14229=CARTESIAN_POINT('Ctrl Pts',(1.30734972067592,1.42347183818157,-1.00672880483252));
#14230=CARTESIAN_POINT('Ctrl Pts',(1.31917543061769,1.39539254159618,-0.99134926498299));
#14231=CARTESIAN_POINT('Ctrl Pts',(1.34548213209931,1.35105447038507,-0.955340251466734));
#14232=CARTESIAN_POINT('Ctrl Pts',(1.36172049302549,1.33182222741682,-0.932292094146255));
#14233=CARTESIAN_POINT('Ctrl Pts',(1.39561049050871,1.30629366210296,-0.880751161609748));
#14234=CARTESIAN_POINT('Ctrl Pts',(1.4132207435299,1.3,-0.852229869895948));
#14235=CARTESIAN_POINT('Ctrl Pts',(1.42894191624432,1.3,-0.825));
#14236=CARTESIAN_POINT('',(1.53744468918255,1.55,-0.598968970568895));
#14237=CARTESIAN_POINT('Ctrl Pts',(1.42894191624432,1.3,-0.825));
#14238=CARTESIAN_POINT('Ctrl Pts',(1.44466308895875,1.3,-0.797770130104051));
#14239=CARTESIAN_POINT('Ctrl Pts',(1.46055812562105,1.30629366210296,-0.768258557763731));
#14240=CARTESIAN_POINT('Ctrl Pts',(1.48824888379079,1.33182222741682,-0.713138492740815));
#14241=CARTESIAN_POINT('Ctrl Pts',(1.50008999307766,1.35105447038507,-0.687551581002688));
#14242=CARTESIAN_POINT('Ctrl Pts',(1.51812136280714,1.39539254159618,-0.646764802471698));
#14243=CARTESIAN_POINT('Ctrl Pts',(1.52552758004446,1.42347183818157,-0.628833667319577));
#14244=CARTESIAN_POINT('Ctrl Pts',(1.53516661651472,1.48505200040818,-0.604921184808249));
#14245=CARTESIAN_POINT('Ctrl Pts',(1.53744468918255,1.51855708359447,-0.598968970568895));
#14246=CARTESIAN_POINT('Ctrl Pts',(1.53744468918255,1.55,-0.598968970568895));
#14247=CARTESIAN_POINT('Ctrl Pts',(1.53744468918255,1.55,-0.598968970568895));
#14248=CARTESIAN_POINT('Ctrl Pts',(1.53744468918255,1.58144291640553,-0.598968970568895));
#14249=CARTESIAN_POINT('Ctrl Pts',(1.53516661651472,1.61494799959182,-0.604921184808249));
#14250=CARTESIAN_POINT('Ctrl Pts',(1.52552758004446,1.67652816181843,-0.628833667319577));
#14251=CARTESIAN_POINT('Ctrl Pts',(1.51812136280714,1.70460745840382,-0.646764802471698));
#14252=CARTESIAN_POINT('Ctrl Pts',(1.50008999307766,1.74894552961493,-0.687551581002688));
#14253=CARTESIAN_POINT('Ctrl Pts',(1.48824888379079,1.76817777258318,-0.713138492740815));
#14254=CARTESIAN_POINT('Ctrl Pts',(1.46055812562105,1.79370633789704,-0.768258557763731));
#14255=CARTESIAN_POINT('Ctrl Pts',(1.44466308895875,1.8,-0.797770130104051));
#14256=CARTESIAN_POINT('Ctrl Pts',(1.42894191624432,1.8,-0.825));
#14257=CARTESIAN_POINT('',(0.,1.3,-1.65));
#14258=CARTESIAN_POINT('',(0.,1.8,-1.65));
#14259=CARTESIAN_POINT('Ctrl Pts',(1.38777878078145E-17,1.3,-1.65));
#14260=CARTESIAN_POINT('Ctrl Pts',(0.0314423454288489,1.3,-1.65));
#14261=CARTESIAN_POINT('Ctrl Pts',(0.0649476351123396,1.30629366210296,
-1.64900971937348));
#14262=CARTESIAN_POINT('Ctrl Pts',(0.126528390765307,1.33182222741682,-1.64543058688707));
#14263=CARTESIAN_POINT('Ctrl Pts',(0.154607860978348,1.35105447038507,-1.64289183246942));
#14264=CARTESIAN_POINT('Ctrl Pts',(0.198945932189457,1.39539254159618,-1.63811406745469));
#14265=CARTESIAN_POINT('Ctrl Pts',(0.218177859368546,1.42347183818157,-1.63556247215209));
#14266=CARTESIAN_POINT('Ctrl Pts',(0.243706194926033,1.48505200040818,-1.63195388134767));
#14267=CARTESIAN_POINT('Ctrl Pts',(0.25,1.51855708359447,-1.63095064303001));
#14268=CARTESIAN_POINT('Ctrl Pts',(0.25,1.58144291640553,-1.63095064303001));
#14269=CARTESIAN_POINT('Ctrl Pts',(0.243706194926033,1.61494799959182,-1.63195388134767));
#14270=CARTESIAN_POINT('Ctrl Pts',(0.218177859368546,1.67652816181843,-1.63556247215209));
#14271=CARTESIAN_POINT('Ctrl Pts',(0.198945932189457,1.70460745840382,-1.63811406745469));
#14272=CARTESIAN_POINT('Ctrl Pts',(0.154607860978349,1.74894552961493,-1.64289183246942));
#14273=CARTESIAN_POINT('Ctrl Pts',(0.126528390765307,1.76817777258318,-1.64543058688707));
#14274=CARTESIAN_POINT('Ctrl Pts',(0.0649476351123398,1.79370633789704,
-1.64900971937348));
#14275=CARTESIAN_POINT('Ctrl Pts',(0.031442345428849,1.8,-1.65));
#14276=CARTESIAN_POINT('Ctrl Pts',(7.63278329429795E-17,1.8,-1.65));
#14277=CARTESIAN_POINT('',(-0.25,1.55,-1.63095064303001));
#14278=CARTESIAN_POINT('Ctrl Pts',(9.0205620750794E-17,1.8,-1.65));
#14279=CARTESIAN_POINT('Ctrl Pts',(-0.0314423454288488,1.8,-1.65));
#14280=CARTESIAN_POINT('Ctrl Pts',(-0.0649476351123396,1.79370633789704,
-1.64900971937348));
#14281=CARTESIAN_POINT('Ctrl Pts',(-0.126528390765307,1.76817777258318,
-1.64543058688707));
#14282=CARTESIAN_POINT('Ctrl Pts',(-0.154607860978348,1.74894552961493,
-1.64289183246942));
#14283=CARTESIAN_POINT('Ctrl Pts',(-0.198945932189456,1.70460745840382,
-1.63811406745469));
#14284=CARTESIAN_POINT('Ctrl Pts',(-0.218177859368546,1.67652816181843,
-1.63556247215209));
#14285=CARTESIAN_POINT('Ctrl Pts',(-0.243706194926033,1.61494799959182,
-1.63195388134767));
#14286=CARTESIAN_POINT('Ctrl Pts',(-0.25,1.58144291640553,-1.63095064303001));
#14287=CARTESIAN_POINT('Ctrl Pts',(-0.25,1.55,-1.63095064303001));
#14288=CARTESIAN_POINT('Ctrl Pts',(-0.25,1.55,-1.63095064303001));
#14289=CARTESIAN_POINT('Ctrl Pts',(-0.25,1.51855708359447,-1.63095064303001));
#14290=CARTESIAN_POINT('Ctrl Pts',(-0.243706194926033,1.48505200040818,
-1.63195388134767));
#14291=CARTESIAN_POINT('Ctrl Pts',(-0.218177859368546,1.42347183818157,
-1.63556247215209));
#14292=CARTESIAN_POINT('Ctrl Pts',(-0.198945932189457,1.39539254159618,
-1.63811406745469));
#14293=CARTESIAN_POINT('Ctrl Pts',(-0.154607860978349,1.35105447038507,
-1.64289183246942));
#14294=CARTESIAN_POINT('Ctrl Pts',(-0.126528390765307,1.33182222741682,
-1.64543058688707));
#14295=CARTESIAN_POINT('Ctrl Pts',(-0.0649476351123398,1.30629366210296,
-1.64900971937348));
#14296=CARTESIAN_POINT('Ctrl Pts',(-0.031442345428849,1.3,-1.65));
#14297=CARTESIAN_POINT('Ctrl Pts',(-4.85722573273506E-17,1.3,-1.65));
#14298=CARTESIAN_POINT('',(0.,1.8,1.65));
#14299=CARTESIAN_POINT('',(0.,1.3,1.65));
#14300=CARTESIAN_POINT('Ctrl Pts',(8.32667268468867E-17,1.8,1.65));
#14301=CARTESIAN_POINT('Ctrl Pts',(0.031442345428849,1.8,1.65));
#14302=CARTESIAN_POINT('Ctrl Pts',(0.0649476351123398,1.79370633789704,
1.64900971937348));
#14303=CARTESIAN_POINT('Ctrl Pts',(0.126528390765307,1.76817777258318,1.64543058688707));
#14304=CARTESIAN_POINT('Ctrl Pts',(0.154607860978349,1.74894552961493,1.64289183246942));
#14305=CARTESIAN_POINT('Ctrl Pts',(0.198945932189457,1.70460745840382,1.63811406745469));
#14306=CARTESIAN_POINT('Ctrl Pts',(0.218177859368546,1.67652816181843,1.63556247215209));
#14307=CARTESIAN_POINT('Ctrl Pts',(0.243706194926033,1.61494799959182,1.63195388134767));
#14308=CARTESIAN_POINT('Ctrl Pts',(0.25,1.58144291640553,1.63095064303001));
#14309=CARTESIAN_POINT('Ctrl Pts',(0.25,1.51855708359447,1.63095064303001));
#14310=CARTESIAN_POINT('Ctrl Pts',(0.243706194926033,1.48505200040818,1.63195388134767));
#14311=CARTESIAN_POINT('Ctrl Pts',(0.218177859368546,1.42347183818157,1.63556247215209));
#14312=CARTESIAN_POINT('Ctrl Pts',(0.198945932189457,1.39539254159618,1.63811406745469));
#14313=CARTESIAN_POINT('Ctrl Pts',(0.154607860978348,1.35105447038507,1.64289183246942));
#14314=CARTESIAN_POINT('Ctrl Pts',(0.126528390765307,1.33182222741682,1.64543058688707));
#14315=CARTESIAN_POINT('Ctrl Pts',(0.0649476351123397,1.30629366210296,
1.64900971937348));
#14316=CARTESIAN_POINT('Ctrl Pts',(0.0314423454288488,1.3,1.65));
#14317=CARTESIAN_POINT('Ctrl Pts',(-1.38777878078145E-17,1.3,1.65));
#14318=CARTESIAN_POINT('',(-0.25,1.55,1.63095064303001));
#14319=CARTESIAN_POINT('Ctrl Pts',(-5.55111512312578E-17,1.3,1.65));
#14320=CARTESIAN_POINT('Ctrl Pts',(-0.031442345428849,1.3,1.65));
#14321=CARTESIAN_POINT('Ctrl Pts',(-0.0649476351123398,1.30629366210296,
1.64900971937348));
#14322=CARTESIAN_POINT('Ctrl Pts',(-0.126528390765307,1.33182222741682,
1.64543058688707));
#14323=CARTESIAN_POINT('Ctrl Pts',(-0.154607860978349,1.35105447038507,
1.64289183246942));
#14324=CARTESIAN_POINT('Ctrl Pts',(-0.198945932189457,1.39539254159618,
1.63811406745469));
#14325=CARTESIAN_POINT('Ctrl Pts',(-0.218177859368546,1.42347183818157,
1.63556247215209));
#14326=CARTESIAN_POINT('Ctrl Pts',(-0.243706194926033,1.48505200040818,
1.63195388134767));
#14327=CARTESIAN_POINT('Ctrl Pts',(-0.25,1.51855708359447,1.63095064303001));
#14328=CARTESIAN_POINT('Ctrl Pts',(-0.25,1.55,1.63095064303001));
#14329=CARTESIAN_POINT('Ctrl Pts',(-0.25,1.55,1.63095064303001));
#14330=CARTESIAN_POINT('Ctrl Pts',(-0.25,1.58144291640553,1.63095064303001));
#14331=CARTESIAN_POINT('Ctrl Pts',(-0.243706194926033,1.61494799959182,
1.63195388134767));
#14332=CARTESIAN_POINT('Ctrl Pts',(-0.218177859368546,1.67652816181843,
1.63556247215209));
#14333=CARTESIAN_POINT('Ctrl Pts',(-0.198945932189456,1.70460745840382,
1.63811406745469));
#14334=CARTESIAN_POINT('Ctrl Pts',(-0.154607860978348,1.74894552961493,
1.64289183246942));
#14335=CARTESIAN_POINT('Ctrl Pts',(-0.126528390765307,1.76817777258318,
1.64543058688707));
#14336=CARTESIAN_POINT('Ctrl Pts',(-0.0649476351123396,1.79370633789704,
1.64900971937348));
#14337=CARTESIAN_POINT('Ctrl Pts',(-0.0314423454288488,1.8,1.65));
#14338=CARTESIAN_POINT('Ctrl Pts',(7.63278329429795E-17,1.8,1.65));
#14339=CARTESIAN_POINT('Origin',(0.,1.55,0.));
#14340=CARTESIAN_POINT('',(-0.713525491562421,1.55,0.700629269222037));
#14341=CARTESIAN_POINT('',(0.125,1.55,0.21650635094611));
#14342=CARTESIAN_POINT('Ctrl Pts',(-0.713525491562421,1.55,0.700629269222037));
#14343=CARTESIAN_POINT('Ctrl Pts',(-0.713525491562421,1.5815373526696,0.700629269222037));
#14344=CARTESIAN_POINT('Ctrl Pts',(-0.718163997970498,1.61508042700263,
0.695997784676727));
#14345=CARTESIAN_POINT('Ctrl Pts',(-0.73619249062986,1.67663267125761,0.676899590973058));
#14346=CARTESIAN_POINT('Ctrl Pts',(-0.749495710301795,1.70465411363682,
0.662390652284073));
#14347=CARTESIAN_POINT('Ctrl Pts',(-0.778498278845144,1.74889618382539,
0.628048950774009));
#14348=CARTESIAN_POINT('Ctrl Pts',(-0.796153444118959,1.76811531482682,
0.605884303066698));
#14349=CARTESIAN_POINT('Ctrl Pts',(-0.832065554235658,1.79367084275751,
0.555538485325663));
#14350=CARTESIAN_POINT('Ctrl Pts',(-0.850258932191534,1.8,0.527308329855002));
#14351=CARTESIAN_POINT('Ctrl Pts',(-0.881791875377343,1.8,0.472691670144998));
#14352=CARTESIAN_POINT('Ctrl Pts',(-0.897143218189782,1.79367084275751,
0.442820664919227));
#14353=CARTESIAN_POINT('Ctrl Pts',(-0.92278792026947,1.76811531482682,0.386546956384144));
#14354=CARTESIAN_POINT('Ctrl Pts',(-0.933155485613026,1.74889618382539,
0.360174810895352));
#14355=CARTESIAN_POINT('Ctrl Pts',(-0.948394987258249,1.70465411363682,
0.31788699900678));
#14356=CARTESIAN_POINT('Ctrl Pts',(-0.954308486908894,1.67663267125761,
0.299111603474267));
#14357=CARTESIAN_POINT('Ctrl Pts',(-0.961833761492987,1.61508042700263,
0.273949373987484));
#14358=CARTESIAN_POINT('Ctrl Pts',(-0.963525491562421,1.5815373526696,0.267616567329817));
#14359=CARTESIAN_POINT('Ctrl Pts',(-0.963525491562421,1.5184626473304,0.267616567329817));
#14360=CARTESIAN_POINT('Ctrl Pts',(-0.961833761492987,1.48491957299737,
0.273949373987484));
#14361=CARTESIAN_POINT('Ctrl Pts',(-0.954308486908894,1.42336732874239,
0.299111603474267));
#14362=CARTESIAN_POINT('Ctrl Pts',(-0.948394987258249,1.39534588636318,
0.31788699900678));
#14363=CARTESIAN_POINT('Ctrl Pts',(-0.933155485613026,1.35110381617461,
0.360174810895352));
#14364=CARTESIAN_POINT('Ctrl Pts',(-0.92278792026947,1.33188468517318,0.386546956384144));
#14365=CARTESIAN_POINT('Ctrl Pts',(-0.897143218189782,1.30632915724249,
0.442820664919227));
#14366=CARTESIAN_POINT('Ctrl Pts',(-0.881791875377343,1.3,0.472691670144998));
#14367=CARTESIAN_POINT('Ctrl Pts',(-0.850258932191534,1.3,0.527308329855002));
#14368=CARTESIAN_POINT('Ctrl Pts',(-0.832065554235658,1.30632915724249,
0.555538485325663));
#14369=CARTESIAN_POINT('Ctrl Pts',(-0.796153444118959,1.33188468517318,
0.605884303066698));
#14370=CARTESIAN_POINT('Ctrl Pts',(-0.778498278845144,1.35110381617461,
0.628048950774009));
#14371=CARTESIAN_POINT('Ctrl Pts',(-0.749495710301795,1.39534588636318,
0.662390652284073));
#14372=CARTESIAN_POINT('Ctrl Pts',(-0.73619249062986,1.42336732874239,0.676899590973058));
#14373=CARTESIAN_POINT('Ctrl Pts',(-0.718163997970498,1.48491957299737,
0.695997784676727));
#14374=CARTESIAN_POINT('Ctrl Pts',(-0.713525491562421,1.5184626473304,0.700629269222037));
#14375=CARTESIAN_POINT('Ctrl Pts',(-0.713525491562421,1.55,0.700629269222037));
#14376=CARTESIAN_POINT('Origin',(0.,1.55,0.));
#14377=CARTESIAN_POINT('',(0.963525491562421,1.55,-0.267616567329817));
#14378=CARTESIAN_POINT('Ctrl Pts',(0.963525491562421,1.55,-0.267616567329817));
#14379=CARTESIAN_POINT('Ctrl Pts',(0.963525491562421,1.5184626473304,-0.267616567329817));
#14380=CARTESIAN_POINT('Ctrl Pts',(0.961833761492987,1.48491957299737,-0.273949373987484));
#14381=CARTESIAN_POINT('Ctrl Pts',(0.954308486908894,1.42336732874239,-0.299111603474267));
#14382=CARTESIAN_POINT('Ctrl Pts',(0.948394987258249,1.39534588636318,-0.31788699900678));
#14383=CARTESIAN_POINT('Ctrl Pts',(0.933155485613026,1.35110381617461,-0.360174810895352));
#14384=CARTESIAN_POINT('Ctrl Pts',(0.92278792026947,1.33188468517318,-0.386546956384144));
#14385=CARTESIAN_POINT('Ctrl Pts',(0.897143218189782,1.30632915724249,-0.442820664919227));
#14386=CARTESIAN_POINT('Ctrl Pts',(0.881791875377343,1.3,-0.472691670144998));
#14387=CARTESIAN_POINT('Ctrl Pts',(0.850258932191534,1.3,-0.527308329855002));
#14388=CARTESIAN_POINT('Ctrl Pts',(0.832065554235658,1.30632915724249,-0.555538485325663));
#14389=CARTESIAN_POINT('Ctrl Pts',(0.796153444118959,1.33188468517318,-0.605884303066698));
#14390=CARTESIAN_POINT('Ctrl Pts',(0.778498278845144,1.35110381617461,-0.628048950774009));
#14391=CARTESIAN_POINT('Ctrl Pts',(0.749495710301795,1.39534588636318,-0.662390652284073));
#14392=CARTESIAN_POINT('Ctrl Pts',(0.73619249062986,1.42336732874239,-0.676899590973058));
#14393=CARTESIAN_POINT('Ctrl Pts',(0.718163997970498,1.48491957299737,-0.695997784676727));
#14394=CARTESIAN_POINT('Ctrl Pts',(0.713525491562421,1.5184626473304,-0.700629269222037));
#14395=CARTESIAN_POINT('Ctrl Pts',(0.713525491562421,1.5815373526696,-0.700629269222037));
#14396=CARTESIAN_POINT('Ctrl Pts',(0.718163997970498,1.61508042700263,-0.695997784676727));
#14397=CARTESIAN_POINT('Ctrl Pts',(0.73619249062986,1.67663267125761,-0.676899590973058));
#14398=CARTESIAN_POINT('Ctrl Pts',(0.749495710301795,1.70465411363682,-0.662390652284073));
#14399=CARTESIAN_POINT('Ctrl Pts',(0.778498278845144,1.74889618382539,-0.628048950774009));
#14400=CARTESIAN_POINT('Ctrl Pts',(0.796153444118959,1.76811531482682,-0.605884303066698));
#14401=CARTESIAN_POINT('Ctrl Pts',(0.832065554235658,1.79367084275751,-0.555538485325663));
#14402=CARTESIAN_POINT('Ctrl Pts',(0.850258932191534,1.8,-0.527308329855002));
#14403=CARTESIAN_POINT('Ctrl Pts',(0.881791875377343,1.8,-0.472691670144998));
#14404=CARTESIAN_POINT('Ctrl Pts',(0.897143218189782,1.79367084275751,-0.442820664919227));
#14405=CARTESIAN_POINT('Ctrl Pts',(0.92278792026947,1.76811531482682,-0.386546956384144));
#14406=CARTESIAN_POINT('Ctrl Pts',(0.933155485613026,1.74889618382539,-0.360174810895352));
#14407=CARTESIAN_POINT('Ctrl Pts',(0.948394987258249,1.70465411363682,-0.31788699900678));
#14408=CARTESIAN_POINT('Ctrl Pts',(0.954308486908894,1.67663267125761,-0.299111603474267));
#14409=CARTESIAN_POINT('Ctrl Pts',(0.961833761492987,1.61508042700263,-0.273949373987484));
#14410=CARTESIAN_POINT('Ctrl Pts',(0.963525491562421,1.5815373526696,-0.267616567329817));
#14411=CARTESIAN_POINT('Ctrl Pts',(0.963525491562421,1.55,-0.267616567329817));
#14412=CARTESIAN_POINT('',(0.125,1.55,0.21650635094611));
#14413=CARTESIAN_POINT('Origin',(0.,1.55,0.));
#14414=CARTESIAN_POINT('',(-0.25,1.55,-0.968245836551854));
#14415=CARTESIAN_POINT('',(-0.25,1.55,0.));
#14416=CARTESIAN_POINT('Ctrl Pts',(-0.25,1.55,-0.968245836551854));
#14417=CARTESIAN_POINT('Ctrl Pts',(-0.25,1.5815373526696,-0.968245836551854));
#14418=CARTESIAN_POINT('Ctrl Pts',(-0.243669763522489,1.61508042700263,
-0.969947158664211));
#14419=CARTESIAN_POINT('Ctrl Pts',(-0.218115996279034,1.67663267125761,
-0.976011194447325));
#14420=CARTESIAN_POINT('Ctrl Pts',(-0.198899276956455,1.70465411363682,
-0.980277651290853));
#14421=CARTESIAN_POINT('Ctrl Pts',(-0.154657206767882,1.74889618382539,
-0.988223761669361));
#14422=CARTESIAN_POINT('Ctrl Pts',(-0.126634476150511,1.76811531482682,
-0.992431259450842));
#14423=CARTESIAN_POINT('Ctrl Pts',(-0.0650776639541238,1.79367084275751,
-0.99835915024489));
#14424=CARTESIAN_POINT('Ctrl Pts',(-0.0315329431858092,1.8,-1.));
#14425=CARTESIAN_POINT('Ctrl Pts',(0.0315329431858092,1.8,-1.));
#14426=CARTESIAN_POINT('Ctrl Pts',(0.0650776639541238,1.79367084275751,
-0.99835915024489));
#14427=CARTESIAN_POINT('Ctrl Pts',(0.126634476150511,1.76811531482682,-0.992431259450842));
#14428=CARTESIAN_POINT('Ctrl Pts',(0.154657206767882,1.74889618382539,-0.988223761669361));
#14429=CARTESIAN_POINT('Ctrl Pts',(0.198899276956455,1.70465411363682,-0.980277651290853));
#14430=CARTESIAN_POINT('Ctrl Pts',(0.218115996279034,1.67663267125761,-0.976011194447325));
#14431=CARTESIAN_POINT('Ctrl Pts',(0.243669763522488,1.61508042700263,-0.969947158664211));
#14432=CARTESIAN_POINT('Ctrl Pts',(0.25,1.5815373526696,-0.968245836551854));
#14433=CARTESIAN_POINT('Ctrl Pts',(0.25,1.5184626473304,-0.968245836551854));
#14434=CARTESIAN_POINT('Ctrl Pts',(0.243669763522488,1.48491957299737,-0.969947158664211));
#14435=CARTESIAN_POINT('Ctrl Pts',(0.218115996279034,1.42336732874239,-0.976011194447325));
#14436=CARTESIAN_POINT('Ctrl Pts',(0.198899276956455,1.39534588636318,-0.980277651290853));
#14437=CARTESIAN_POINT('Ctrl Pts',(0.154657206767882,1.35110381617461,-0.988223761669361));
#14438=CARTESIAN_POINT('Ctrl Pts',(0.126634476150511,1.33188468517318,-0.992431259450842));
#14439=CARTESIAN_POINT('Ctrl Pts',(0.0650776639541239,1.30632915724249,
-0.99835915024489));
#14440=CARTESIAN_POINT('Ctrl Pts',(0.0315329431858092,1.3,-1.));
#14441=CARTESIAN_POINT('Ctrl Pts',(-0.0315329431858092,1.3,-1.));
#14442=CARTESIAN_POINT('Ctrl Pts',(-0.0650776639541239,1.30632915724249,
-0.99835915024489));
#14443=CARTESIAN_POINT('Ctrl Pts',(-0.126634476150511,1.33188468517318,
-0.992431259450842));
#14444=CARTESIAN_POINT('Ctrl Pts',(-0.154657206767882,1.35110381617461,
-0.988223761669361));
#14445=CARTESIAN_POINT('Ctrl Pts',(-0.198899276956455,1.39534588636318,
-0.980277651290853));
#14446=CARTESIAN_POINT('Ctrl Pts',(-0.218115996279034,1.42336732874239,
-0.976011194447325));
#14447=CARTESIAN_POINT('Ctrl Pts',(-0.243669763522489,1.48491957299737,
-0.969947158664211));
#14448=CARTESIAN_POINT('Ctrl Pts',(-0.25,1.5184626473304,-0.968245836551854));
#14449=CARTESIAN_POINT('Ctrl Pts',(-0.25,1.55,-0.968245836551854));
#14450=CARTESIAN_POINT('Origin',(0.,1.55,0.));
#14451=CARTESIAN_POINT('',(-0.25,1.55,0.968245836551854));
#14452=CARTESIAN_POINT('Ctrl Pts',(-0.25,1.55,0.968245836551854));
#14453=CARTESIAN_POINT('Ctrl Pts',(-0.25,1.5184626473304,0.968245836551854));
#14454=CARTESIAN_POINT('Ctrl Pts',(-0.243669763522489,1.48491957299737,
0.969947158664211));
#14455=CARTESIAN_POINT('Ctrl Pts',(-0.218115996279034,1.42336732874239,
0.976011194447325));
#14456=CARTESIAN_POINT('Ctrl Pts',(-0.198899276956455,1.39534588636318,
0.980277651290853));
#14457=CARTESIAN_POINT('Ctrl Pts',(-0.154657206767882,1.35110381617461,
0.988223761669361));
#14458=CARTESIAN_POINT('Ctrl Pts',(-0.126634476150511,1.33188468517318,
0.992431259450842));
#14459=CARTESIAN_POINT('Ctrl Pts',(-0.065077663954124,1.30632915724249,
0.99835915024489));
#14460=CARTESIAN_POINT('Ctrl Pts',(-0.0315329431858092,1.3,1.));
#14461=CARTESIAN_POINT('Ctrl Pts',(0.0315329431858092,1.3,1.));
#14462=CARTESIAN_POINT('Ctrl Pts',(0.065077663954124,1.30632915724249,0.99835915024489));
#14463=CARTESIAN_POINT('Ctrl Pts',(0.126634476150511,1.33188468517318,0.992431259450842));
#14464=CARTESIAN_POINT('Ctrl Pts',(0.154657206767882,1.35110381617461,0.988223761669361));
#14465=CARTESIAN_POINT('Ctrl Pts',(0.198899276956455,1.39534588636318,0.980277651290853));
#14466=CARTESIAN_POINT('Ctrl Pts',(0.218115996279034,1.42336732874239,0.976011194447325));
#14467=CARTESIAN_POINT('Ctrl Pts',(0.243669763522488,1.48491957299737,0.969947158664211));
#14468=CARTESIAN_POINT('Ctrl Pts',(0.25,1.5184626473304,0.968245836551854));
#14469=CARTESIAN_POINT('Ctrl Pts',(0.25,1.5815373526696,0.968245836551854));
#14470=CARTESIAN_POINT('Ctrl Pts',(0.243669763522488,1.61508042700263,0.969947158664211));
#14471=CARTESIAN_POINT('Ctrl Pts',(0.218115996279034,1.67663267125761,0.976011194447325));
#14472=CARTESIAN_POINT('Ctrl Pts',(0.198899276956455,1.70465411363682,0.980277651290853));
#14473=CARTESIAN_POINT('Ctrl Pts',(0.154657206767882,1.74889618382539,0.988223761669361));
#14474=CARTESIAN_POINT('Ctrl Pts',(0.126634476150511,1.76811531482682,0.992431259450842));
#14475=CARTESIAN_POINT('Ctrl Pts',(0.0650776639541239,1.79367084275751,
0.99835915024489));
#14476=CARTESIAN_POINT('Ctrl Pts',(0.0315329431858092,1.8,1.));
#14477=CARTESIAN_POINT('Ctrl Pts',(-0.0315329431858092,1.8,1.));
#14478=CARTESIAN_POINT('Ctrl Pts',(-0.0650776639541239,1.79367084275751,
0.99835915024489));
#14479=CARTESIAN_POINT('Ctrl Pts',(-0.126634476150511,1.76811531482682,
0.992431259450842));
#14480=CARTESIAN_POINT('Ctrl Pts',(-0.154657206767882,1.74889618382539,
0.988223761669361));
#14481=CARTESIAN_POINT('Ctrl Pts',(-0.198899276956455,1.70465411363682,
0.980277651290853));
#14482=CARTESIAN_POINT('Ctrl Pts',(-0.218115996279034,1.67663267125761,
0.976011194447325));
#14483=CARTESIAN_POINT('Ctrl Pts',(-0.243669763522489,1.61508042700263,
0.969947158664211));
#14484=CARTESIAN_POINT('Ctrl Pts',(-0.25,1.5815373526696,0.968245836551854));
#14485=CARTESIAN_POINT('Ctrl Pts',(-0.25,1.55,0.968245836551854));
#14486=CARTESIAN_POINT('',(-0.25,1.55,0.));
#14487=CARTESIAN_POINT('Origin',(1.65,2.25,0.));
#14488=CARTESIAN_POINT('',(-1.,2.25,-1.22464679914735E-16));
#14489=CARTESIAN_POINT('Origin',(0.,2.25,0.));
#14490=CARTESIAN_POINT('Origin',(1.75,0.85,0.));
#14491=CARTESIAN_POINT('',(-1.75,0.85,-2.14313189850787E-16));
#14492=CARTESIAN_POINT('Origin',(0.,0.85,0.));
#14493=CARTESIAN_POINT('Origin',(0.,0.,0.));
#14494=CARTESIAN_POINT('',(-1.75,-0.85,-2.14313189850787E-16));
#14495=CARTESIAN_POINT('Origin',(0.,-0.85,0.));
#14496=CARTESIAN_POINT('',(-1.75,0.,-2.14313189850787E-16));
#14497=CARTESIAN_POINT('Origin',(1.,-0.85,0.));
#14498=CARTESIAN_POINT('',(-1.,-0.85,-1.22464679914735E-16));
#14499=CARTESIAN_POINT('Origin',(0.,-0.85,0.));
#14500=CARTESIAN_POINT('Origin',(0.,0.7,0.));
#14501=CARTESIAN_POINT('',(-1.,0.7,-1.22464679914735E-16));
#14502=CARTESIAN_POINT('',(0.,0.,0.));
#14503=CARTESIAN_POINT('',(0.,0.,0.));
#14504=CARTESIAN_POINT('',(0.,0.,0.));
#14505=CARTESIAN_POINT('Origin',(0.,0.,0.));
#14506=CARTESIAN_POINT('',(-0.42,0.16,5.14351655641888E-17));
#14507=CARTESIAN_POINT('Origin',(0.,0.16,0.));
#14508=CARTESIAN_POINT('',(-0.42,0.,5.14351655641888E-17));
#14509=CARTESIAN_POINT('',(-0.42,0.,5.14351655641888E-17));
#14510=CARTESIAN_POINT('Origin',(0.,0.,0.));
#14511=CARTESIAN_POINT('Origin',(0.,0.,0.));
#14512=CARTESIAN_POINT('',(-0.8,0.16,9.79717439317883E-17));
#14513=CARTESIAN_POINT('Origin',(0.,0.16,0.));
#14514=CARTESIAN_POINT('',(-0.8,0.,9.79717439317883E-17));
#14515=CARTESIAN_POINT('',(-0.8,0.,9.79717439317883E-17));
#14516=CARTESIAN_POINT('Origin',(0.,0.,0.));
#14517=CARTESIAN_POINT('Origin',(0.,0.16,0.));
#14518=CARTESIAN_POINT('Origin',(0.,0.,0.));
#14519=CARTESIAN_POINT('',(0.,0.,0.));
#14520=CARTESIAN_POINT('Origin',(0.173205080756888,-0.8,-0.3));
#14521=CARTESIAN_POINT('',(0.346410161513775,-0.8,0.));
#14522=CARTESIAN_POINT('',(0.173205080756888,-0.8,-0.3));
#14523=CARTESIAN_POINT('',(0.346410161513775,-0.8,0.));
#14524=CARTESIAN_POINT('',(0.173205080756888,-1.28,-0.3));
#14525=CARTESIAN_POINT('',(0.173205080756888,-0.8,-0.3));
#14526=CARTESIAN_POINT('',(0.346410161513775,-1.28,0.));
#14527=CARTESIAN_POINT('',(0.346410161513775,-1.28,0.));
#14528=CARTESIAN_POINT('',(0.346410161513775,-0.8,0.));
#14529=CARTESIAN_POINT('Origin',(-0.173205080756888,-0.8,-0.3));
#14530=CARTESIAN_POINT('',(-0.173205080756888,-0.8,-0.3));
#14531=CARTESIAN_POINT('',(0.173205080756888,-0.8,-0.3));
#14532=CARTESIAN_POINT('',(-0.173205080756888,-1.28,-0.3));
#14533=CARTESIAN_POINT('',(-0.173205080756888,-0.8,-0.3));
#14534=CARTESIAN_POINT('',(0.173205080756888,-1.28,-0.3));
#14535=CARTESIAN_POINT('Origin',(-0.346410161513775,-0.8,-5.55111512312578E-17));
#14536=CARTESIAN_POINT('',(-0.346410161513775,-0.8,-4.24230095489963E-17));
#14537=CARTESIAN_POINT('',(-0.173205080756888,-0.8,-0.3));
#14538=CARTESIAN_POINT('',(-0.346410161513775,-1.28,-5.55111512312578E-17));
#14539=CARTESIAN_POINT('',(-0.346410161513775,-0.8,-4.24230095489963E-17));
#14540=CARTESIAN_POINT('',(-0.173205080756888,-1.28,-0.3));
#14541=CARTESIAN_POINT('Origin',(-0.173205080756888,-0.8,0.3));
#14542=CARTESIAN_POINT('',(-0.173205080756888,-0.8,0.3));
#14543=CARTESIAN_POINT('',(-0.346410161513775,-0.8,-4.24230095489963E-17));
#14544=CARTESIAN_POINT('',(-0.173205080756888,-1.28,0.3));
#14545=CARTESIAN_POINT('',(-0.173205080756888,-0.8,0.3));
#14546=CARTESIAN_POINT('',(-0.346410161513775,-1.28,-4.24230095489963E-17));
#14547=CARTESIAN_POINT('Origin',(0.173205080756888,-0.8,0.3));
#14548=CARTESIAN_POINT('',(0.173205080756888,-0.8,0.3));
#14549=CARTESIAN_POINT('',(-0.173205080756888,-0.8,0.3));
#14550=CARTESIAN_POINT('',(0.173205080756888,-1.28,0.3));
#14551=CARTESIAN_POINT('',(0.173205080756888,-0.8,0.3));
#14552=CARTESIAN_POINT('',(-0.173205080756888,-1.28,0.3));
#14553=CARTESIAN_POINT('Origin',(0.346410161513775,-0.8,0.));
#14554=CARTESIAN_POINT('',(0.173205080756888,-0.8,0.3));
#14555=CARTESIAN_POINT('',(0.173205080756888,-1.28,0.3));
#14556=CARTESIAN_POINT('Origin',(0.,-0.8,-5.55111512312578E-17));
#14557=CARTESIAN_POINT('Origin',(0.,-1.28,-5.55111512312578E-17));
#14558=CARTESIAN_POINT('Origin',(0.,-2.5,0.));
#14559=CARTESIAN_POINT('',(-0.3933,-2.5,4.81653586104654E-17));
#14560=CARTESIAN_POINT('Origin',(0.,-2.5,0.));
#14561=CARTESIAN_POINT('Origin',(0.6,0.8,0.));
#14562=CARTESIAN_POINT('',(-0.6,0.8,-7.34788079488412E-17));
#14563=CARTESIAN_POINT('Origin',(0.,0.8,0.));
#14564=CARTESIAN_POINT('Origin',(0.,0.775,0.));
#14565=CARTESIAN_POINT('',(-0.65,0.75,-7.9602041944578E-17));
#14566=CARTESIAN_POINT('Origin',(0.,0.75,0.));
#14567=CARTESIAN_POINT('',(-0.625,0.775,-7.65404249467096E-17));
#14568=CARTESIAN_POINT('Origin',(0.,0.39,0.));
#14569=CARTESIAN_POINT('',(-0.65,0.0299999999999998,-7.9602041944578E-17));
#14570=CARTESIAN_POINT('Origin',(0.,0.0299999999999998,0.));
#14571=CARTESIAN_POINT('',(-0.65,0.39,-7.9602041944578E-17));
#14572=CARTESIAN_POINT('Origin',(0.,0.0150000000000001,0.));
#14573=CARTESIAN_POINT('',(-0.62,5.89805981832114E-17,-7.59281015471359E-17));
#14574=CARTESIAN_POINT('Origin',(0.,0.,0.));
#14575=CARTESIAN_POINT('',(-0.635,0.0150000000000001,-7.77650717458569E-17));
#14576=CARTESIAN_POINT('Origin',(0.42,0.,0.));
#14577=CARTESIAN_POINT('',(-0.42,-3.46944695195361E-18,-5.14351655641888E-17));
#14578=CARTESIAN_POINT('Origin',(0.,0.,0.));
#14579=CARTESIAN_POINT('Origin',(0.,-0.02,0.));
#14580=CARTESIAN_POINT('',(-0.3933,-0.0534000000000001,4.81653586104654E-17));
#14581=CARTESIAN_POINT('Origin',(0.,-0.0534000000000001,0.));
#14582=CARTESIAN_POINT('',(-0.41,-0.02,-5.02105187650415E-17));
#14583=CARTESIAN_POINT('Origin',(0.,-1.48,0.));
#14584=CARTESIAN_POINT('',(-0.3933,-1.48,-4.81653586104654E-17));
#14585=CARTESIAN_POINT('',(0.,0.,0.));
#14586=CARTESIAN_POINT('Origin',(14.,0.,0.97));
#14587=CARTESIAN_POINT('',(13.625,-4.59242549680257E-17,0.97));
#14588=CARTESIAN_POINT('Origin',(14.,0.,0.97));
#14589=CARTESIAN_POINT('',(13.625,4.59242549680257E-17,1.5));
#14590=CARTESIAN_POINT('',(13.625,-4.59242549680257E-17,0.97));
#14591=CARTESIAN_POINT('Origin',(14.,0.,1.5));
#14592=CARTESIAN_POINT('Origin',(14.,0.,0.97));
#14593=CARTESIAN_POINT('',(13.775,-2.75545529808154E-17,0.97));
#14594=CARTESIAN_POINT('Origin',(14.,0.,0.97));
#14595=CARTESIAN_POINT('Origin',(8.,0.,0.97));
#14596=CARTESIAN_POINT('',(7.625,-4.59242549680257E-17,0.97));
#14597=CARTESIAN_POINT('Origin',(8.,0.,0.97));
#14598=CARTESIAN_POINT('',(7.625,4.59242549680257E-17,1.5));
#14599=CARTESIAN_POINT('',(7.625,-4.59242549680257E-17,0.97));
#14600=CARTESIAN_POINT('Origin',(8.,0.,1.5));
#14601=CARTESIAN_POINT('Origin',(8.,0.,0.97));
#14602=CARTESIAN_POINT('',(7.775,-2.75545529808154E-17,0.97));
#14603=CARTESIAN_POINT('Origin',(8.,0.,0.97));
#14604=CARTESIAN_POINT('Origin',(2.,0.,0.97));
#14605=CARTESIAN_POINT('',(1.625,-4.59242549680257E-17,0.97));
#14606=CARTESIAN_POINT('Origin',(2.,0.,0.97));
#14607=CARTESIAN_POINT('',(1.625,4.59242549680257E-17,1.5));
#14608=CARTESIAN_POINT('',(1.625,-4.59242549680257E-17,0.97));
#14609=CARTESIAN_POINT('Origin',(2.,0.,1.5));
#14610=CARTESIAN_POINT('Origin',(2.,0.,0.97));
#14611=CARTESIAN_POINT('',(1.775,-2.75545529808155E-17,0.97));
#14612=CARTESIAN_POINT('Origin',(2.,0.,0.97));
#14613=CARTESIAN_POINT('Origin',(20.,0.,0.97));
#14614=CARTESIAN_POINT('',(19.625,-4.59242549680257E-17,0.97));
#14615=CARTESIAN_POINT('Origin',(20.,0.,0.97));
#14616=CARTESIAN_POINT('',(19.625,4.59242549680257E-17,1.5));
#14617=CARTESIAN_POINT('',(19.625,-4.59242549680257E-17,0.97));
#14618=CARTESIAN_POINT('Origin',(20.,0.,1.5));
#14619=CARTESIAN_POINT('Origin',(20.,0.,0.97));
#14620=CARTESIAN_POINT('',(19.775,-2.75545529808156E-17,0.97));
#14621=CARTESIAN_POINT('Origin',(20.,0.,0.97));
#14622=CARTESIAN_POINT('Origin',(14.,0.,-0.1));
#14623=CARTESIAN_POINT('',(13.775,-2.75545529808154E-17,0.));
#14624=CARTESIAN_POINT('Origin',(14.,0.,0.));
#14625=CARTESIAN_POINT('',(13.775,-2.75545529808154E-17,-0.1));
#14626=CARTESIAN_POINT('Origin',(8.,0.,-0.1));
#14627=CARTESIAN_POINT('',(7.775,-2.75545529808154E-17,0.));
#14628=CARTESIAN_POINT('Origin',(8.,0.,0.));
#14629=CARTESIAN_POINT('',(7.775,-2.75545529808154E-17,-0.1));
#14630=CARTESIAN_POINT('Origin',(2.,0.,-0.1));
#14631=CARTESIAN_POINT('',(1.775,-2.75545529808155E-17,0.));
#14632=CARTESIAN_POINT('Origin',(2.,0.,0.));
#14633=CARTESIAN_POINT('',(1.775,-2.75545529808155E-17,-0.1));
#14634=CARTESIAN_POINT('Origin',(20.,0.,-0.1));
#14635=CARTESIAN_POINT('',(19.775,-2.75545529808156E-17,0.));
#14636=CARTESIAN_POINT('Origin',(20.,0.,0.));
#14637=CARTESIAN_POINT('',(19.775,-2.75545529808156E-17,-0.1));
#14638=CARTESIAN_POINT('Origin',(0.,-0.53,1.));
#14639=CARTESIAN_POINT('',(0.,-0.53,1.));
#14640=CARTESIAN_POINT('',(0.,-0.75,0.85));
#14641=CARTESIAN_POINT('',(0.,-0.53,1.));
#14642=CARTESIAN_POINT('',(22.,-0.75,0.85));
#14643=CARTESIAN_POINT('',(0.,-0.75,0.85));
#14644=CARTESIAN_POINT('',(22.,-0.53,1.));
#14645=CARTESIAN_POINT('',(22.,-0.53,1.));
#14646=CARTESIAN_POINT('',(0.,-0.53,1.));
#14647=CARTESIAN_POINT('Origin',(0.,-0.53,1.15));
#14648=CARTESIAN_POINT('',(0.,-0.53,1.15));
#14649=CARTESIAN_POINT('',(0.,-0.53,1.15));
#14650=CARTESIAN_POINT('',(22.,-0.53,1.15));
#14651=CARTESIAN_POINT('',(22.,-0.53,1.15));
#14652=CARTESIAN_POINT('',(0.,-0.53,1.15));
#14653=CARTESIAN_POINT('Origin',(0.,-0.75,1.3));
#14654=CARTESIAN_POINT('',(0.,-0.75,1.3));
#14655=CARTESIAN_POINT('',(0.,-0.75,1.3));
#14656=CARTESIAN_POINT('',(22.,-0.75,1.3));
#14657=CARTESIAN_POINT('',(22.,-0.75,1.3));
#14658=CARTESIAN_POINT('',(0.,-0.75,1.3));
#14659=CARTESIAN_POINT('Origin',(0.,-0.75,1.5));
#14660=CARTESIAN_POINT('',(0.,-0.75,1.5));
#14661=CARTESIAN_POINT('',(0.,-0.75,1.5));
#14662=CARTESIAN_POINT('',(22.,-0.75,1.5));
#14663=CARTESIAN_POINT('',(22.,-0.75,1.5));
#14664=CARTESIAN_POINT('',(0.,-0.75,1.5));
#14665=CARTESIAN_POINT('Origin',(0.,0.75,1.5));
#14666=CARTESIAN_POINT('',(0.,0.75,1.5));
#14667=CARTESIAN_POINT('',(0.,0.75,1.5));
#14668=CARTESIAN_POINT('',(22.,0.75,1.5));
#14669=CARTESIAN_POINT('',(22.,0.75,1.5));
#14670=CARTESIAN_POINT('',(0.,0.75,1.5));
#14671=CARTESIAN_POINT('Origin',(0.,0.75,1.3));
#14672=CARTESIAN_POINT('',(0.,0.75,1.3));
#14673=CARTESIAN_POINT('',(0.,0.75,1.3));
#14674=CARTESIAN_POINT('',(22.,0.75,1.3));
#14675=CARTESIAN_POINT('',(22.,0.75,1.3));
#14676=CARTESIAN_POINT('',(0.,0.75,1.3));
#14677=CARTESIAN_POINT('Origin',(0.,0.53,1.15));
#14678=CARTESIAN_POINT('',(0.,0.53,1.15));
#14679=CARTESIAN_POINT('',(0.,0.53,1.15));
#14680=CARTESIAN_POINT('',(22.,0.53,1.15));
#14681=CARTESIAN_POINT('',(22.,0.53,1.15));
#14682=CARTESIAN_POINT('',(0.,0.53,1.15));
#14683=CARTESIAN_POINT('Origin',(0.,0.53,1.));
#14684=CARTESIAN_POINT('',(0.,0.53,1.));
#14685=CARTESIAN_POINT('',(0.,0.53,1.));
#14686=CARTESIAN_POINT('',(22.,0.53,1.));
#14687=CARTESIAN_POINT('',(22.,0.53,1.));
#14688=CARTESIAN_POINT('',(0.,0.53,1.));
#14689=CARTESIAN_POINT('Origin',(0.,0.75,0.85));
#14690=CARTESIAN_POINT('',(0.,0.75,0.85));
#14691=CARTESIAN_POINT('',(0.,0.75,0.85));
#14692=CARTESIAN_POINT('',(22.,0.75,0.85));
#14693=CARTESIAN_POINT('',(22.,0.75,0.85));
#14694=CARTESIAN_POINT('',(0.,0.75,0.85));
#14695=CARTESIAN_POINT('Origin',(0.,0.75,0.));
#14696=CARTESIAN_POINT('',(0.,0.75,0.));
#14697=CARTESIAN_POINT('',(0.,0.75,0.));
#14698=CARTESIAN_POINT('',(22.,0.75,0.));
#14699=CARTESIAN_POINT('',(22.,0.75,0.));
#14700=CARTESIAN_POINT('',(0.,0.75,0.));
#14701=CARTESIAN_POINT('Origin',(0.,-0.75,0.));
#14702=CARTESIAN_POINT('',(0.,-0.75,0.));
#14703=CARTESIAN_POINT('',(0.,-0.75,0.));
#14704=CARTESIAN_POINT('',(22.,-0.75,0.));
#14705=CARTESIAN_POINT('',(22.,-0.75,0.));
#14706=CARTESIAN_POINT('',(0.,-0.75,0.));
#14707=CARTESIAN_POINT('Origin',(0.,-0.75,0.85));
#14708=CARTESIAN_POINT('',(0.,-0.75,0.85));
#14709=CARTESIAN_POINT('',(22.,-0.75,0.85));
#14710=CARTESIAN_POINT('Origin',(22.,0.,0.75));
#14711=CARTESIAN_POINT('Origin',(0.,0.,0.75));
#14712=CARTESIAN_POINT('',(0.,0.,0.));
#14713=CARTESIAN_POINT('Origin',(0.3,0.4,0.));
#14714=CARTESIAN_POINT('',(-0.3,0.4,-3.67394039744206E-17));
#14715=CARTESIAN_POINT('Origin',(0.,0.4,0.));
#14716=CARTESIAN_POINT('Origin',(0.,0.375,0.));
#14717=CARTESIAN_POINT('',(-0.35,0.35,-4.28626379701573E-17));
#14718=CARTESIAN_POINT('Origin',(0.,0.35,0.));
#14719=CARTESIAN_POINT('',(-0.325,0.375,-3.9801020972289E-17));
#14720=CARTESIAN_POINT('Origin',(0.,0.19,0.));
#14721=CARTESIAN_POINT('',(-0.35,0.03,-4.28626379701574E-17));
#14722=CARTESIAN_POINT('Origin',(0.,0.03,0.));
#14723=CARTESIAN_POINT('',(-0.35,0.19,-4.28626379701574E-17));
#14724=CARTESIAN_POINT('Origin',(0.,0.0149999999999999,0.));
#14725=CARTESIAN_POINT('',(-0.32,-3.29597460435593E-17,-3.91886975727153E-17));
#14726=CARTESIAN_POINT('Origin',(0.,0.,0.));
#14727=CARTESIAN_POINT('',(-0.335,0.0149999999999999,-4.10256677714363E-17));
#14728=CARTESIAN_POINT('Origin',(0.22,0.,0.));
#14729=CARTESIAN_POINT('',(-0.22,-6.93889390390723E-18,-2.69422295812418E-17));
#14730=CARTESIAN_POINT('Origin',(0.,0.,0.));
#14731=CARTESIAN_POINT('Origin',(0.,-0.02,0.));
#14732=CARTESIAN_POINT('',(-0.1954,-0.0492,2.39295984553393E-17));
#14733=CARTESIAN_POINT('Origin',(0.,-0.0492,0.));
#14734=CARTESIAN_POINT('',(-0.21,-0.02,-2.57175827820944E-17));
#14735=CARTESIAN_POINT('Origin',(0.,-0.8,0.));
#14736=CARTESIAN_POINT('',(-0.1954,-1.5646,2.39295984553393E-17));
#14737=CARTESIAN_POINT('Origin',(0.,-1.5646,0.));
#14738=CARTESIAN_POINT('',(-0.1954,-0.8,-2.39295984553393E-17));
#14739=CARTESIAN_POINT('Origin',(0.,-1.58,0.));
#14740=CARTESIAN_POINT('',(-0.16,-1.6,-1.95943487863577E-17));
#14741=CARTESIAN_POINT('Origin',(0.,-1.6,0.));
#14742=CARTESIAN_POINT('',(-0.18,-1.58,-2.20436423846524E-17));
#14743=CARTESIAN_POINT('Origin',(0.,-1.6,0.));
#14744=CARTESIAN_POINT('Origin',(0.0866025403784439,-0.4,-0.15));
#14745=CARTESIAN_POINT('',(0.173205080756888,-0.4,0.));
#14746=CARTESIAN_POINT('',(0.0866025403784439,-0.4,-0.15));
#14747=CARTESIAN_POINT('',(0.173205080756888,-0.4,0.));
#14748=CARTESIAN_POINT('',(0.0866025403784439,-0.64,-0.15));
#14749=CARTESIAN_POINT('',(0.0866025403784439,-0.4,-0.15));
#14750=CARTESIAN_POINT('',(0.173205080756888,-0.64,0.));
#14751=CARTESIAN_POINT('',(0.173205080756888,-0.64,0.));
#14752=CARTESIAN_POINT('',(0.173205080756888,-0.4,0.));
#14753=CARTESIAN_POINT('Origin',(-0.0866025403784438,-0.4,-0.15));
#14754=CARTESIAN_POINT('',(-0.0866025403784438,-0.4,-0.15));
#14755=CARTESIAN_POINT('',(0.0866025403784439,-0.4,-0.15));
#14756=CARTESIAN_POINT('',(-0.0866025403784438,-0.64,-0.15));
#14757=CARTESIAN_POINT('',(-0.0866025403784438,-0.4,-0.15));
#14758=CARTESIAN_POINT('',(0.0866025403784439,-0.64,-0.15));
#14759=CARTESIAN_POINT('Origin',(-0.173205080756888,-0.4,-2.77555756156289E-17));
#14760=CARTESIAN_POINT('',(-0.173205080756888,-0.4,-2.12115047744981E-17));
#14761=CARTESIAN_POINT('',(-0.0866025403784438,-0.4,-0.15));
#14762=CARTESIAN_POINT('',(-0.173205080756888,-0.64,-2.77555756156289E-17));
#14763=CARTESIAN_POINT('',(-0.173205080756888,-0.4,-2.12115047744981E-17));
#14764=CARTESIAN_POINT('',(-0.0866025403784438,-0.64,-0.15));
#14765=CARTESIAN_POINT('Origin',(-0.0866025403784439,-0.4,0.15));
#14766=CARTESIAN_POINT('',(-0.0866025403784439,-0.4,0.15));
#14767=CARTESIAN_POINT('',(-0.173205080756888,-0.4,-2.12115047744981E-17));
#14768=CARTESIAN_POINT('',(-0.0866025403784439,-0.64,0.15));
#14769=CARTESIAN_POINT('',(-0.0866025403784439,-0.4,0.15));
#14770=CARTESIAN_POINT('',(-0.173205080756888,-0.64,-2.12115047744981E-17));
#14771=CARTESIAN_POINT('Origin',(0.0866025403784439,-0.4,0.15));
#14772=CARTESIAN_POINT('',(0.0866025403784439,-0.4,0.15));
#14773=CARTESIAN_POINT('',(-0.0866025403784439,-0.4,0.15));
#14774=CARTESIAN_POINT('',(0.0866025403784439,-0.64,0.15));
#14775=CARTESIAN_POINT('',(0.0866025403784439,-0.4,0.15));
#14776=CARTESIAN_POINT('',(-0.0866025403784439,-0.64,0.15));
#14777=CARTESIAN_POINT('Origin',(0.173205080756888,-0.4,0.));
#14778=CARTESIAN_POINT('',(0.0866025403784439,-0.4,0.15));
#14779=CARTESIAN_POINT('',(0.0866025403784439,-0.64,0.15));
#14780=CARTESIAN_POINT('Origin',(0.,-0.4,-2.77555756156289E-17));
#14781=CARTESIAN_POINT('Origin',(0.,-0.64,-2.77555756156289E-17));
#14782=CARTESIAN_POINT('',(0.,0.,0.));
#14783=CARTESIAN_POINT('',(0.,0.,0.));
#14784=CARTESIAN_POINT('Origin',(-0.3,-1.5,10.9));
#14785=CARTESIAN_POINT('',(-0.3,0.5,11.0460607985831));
#14786=CARTESIAN_POINT('',(-0.3,-1.5,11.0460607985831));
#14787=CARTESIAN_POINT('',(-0.3,-19.,11.0460607985831));
#14788=CARTESIAN_POINT('',(-0.3,0.5,11.35));
#14789=CARTESIAN_POINT('',(-0.3,0.5,11.45));
#14790=CARTESIAN_POINT('',(-0.3,-1.5,11.35));
#14791=CARTESIAN_POINT('',(-0.3,-1.5,11.35));
#14792=CARTESIAN_POINT('',(-0.3,-1.5,11.35));
#14793=CARTESIAN_POINT('Origin',(0.,-1.5,11.125));
#14794=CARTESIAN_POINT('',(0.3,-1.5,11.0460607985831));
#14795=CARTESIAN_POINT('Origin',(0.,-1.5,12.));
#14796=CARTESIAN_POINT('',(0.3,-1.5,11.35));
#14797=CARTESIAN_POINT('',(0.3,-1.5,11.35));
#14798=CARTESIAN_POINT('',(0.3,-1.5,10.9));
#14799=CARTESIAN_POINT('Origin',(0.3,-1.5,11.35));
#14800=CARTESIAN_POINT('',(0.3,0.5,11.0460607985831));
#14801=CARTESIAN_POINT('',(0.3,-19.,11.0460607985831));
#14802=CARTESIAN_POINT('',(0.3,0.5,11.35));
#14803=CARTESIAN_POINT('',(0.3,-1.5,11.35));
#14804=CARTESIAN_POINT('',(0.3,0.5,11.675));
#14805=CARTESIAN_POINT('Origin',(-0.3,-1.5,11.35));
#14806=CARTESIAN_POINT('',(-0.15,0.5,11.35));
#14807=CARTESIAN_POINT('Origin',(0.,-19.,12.));
#14808=CARTESIAN_POINT('',(-1.,0.5,12.));
#14809=CARTESIAN_POINT('Origin',(0.,0.5,12.));
#14810=CARTESIAN_POINT('',(-1.,-19.,12.));
#14811=CARTESIAN_POINT('',(-1.,-19.,12.));
#14812=CARTESIAN_POINT('Origin',(0.,-19.,12.));
#14813=CARTESIAN_POINT('Origin',(0.,0.5,12.));
#14814=CARTESIAN_POINT('Origin',(0.,0.5,12.));
#14815=CARTESIAN_POINT('Origin',(0.,-19.,12.));
#14816=CARTESIAN_POINT('',(0.,0.,0.));
#14817=CARTESIAN_POINT('Origin',(0.,-17.05,12.99));
#14818=CARTESIAN_POINT('',(0.172988438920051,-17.1690588089979,12.99));
#14819=CARTESIAN_POINT('',(0.172988438920051,-16.9309411910021,12.99));
#14820=CARTESIAN_POINT('',(0.172988438920051,-17.45,12.99));
#14821=CARTESIAN_POINT('Origin',(0.,-17.05,12.99));
#14822=CARTESIAN_POINT('Origin',(0.,-17.05,12.99));
#14823=CARTESIAN_POINT('',(-0.172988438920051,-17.1690588089979,12.99));
#14824=CARTESIAN_POINT('Ctrl Pts',(-0.172988438920049,-17.1690588089979,
12.99));
#14825=CARTESIAN_POINT('Ctrl Pts',(-0.165594865311309,-17.1798014223953,
12.9912919219764));
#14826=CARTESIAN_POINT('Ctrl Pts',(-0.157297138725604,-17.1896877093727,
12.992653949439));
#14827=CARTESIAN_POINT('Ctrl Pts',(-0.129892073845076,-17.2170927742533,
12.9967480843909));
#14828=CARTESIAN_POINT('Ctrl Pts',(-0.106330167759284,-17.233242056333,
12.9996958932764));
#14829=CARTESIAN_POINT('Ctrl Pts',(-0.0546129046324093,-17.2546977939649,
13.0038502947236));
#14830=CARTESIAN_POINT('Ctrl Pts',(-0.0264512308298518,-17.26,13.005));
#14831=CARTESIAN_POINT('Ctrl Pts',(0.0264512308298517,-17.26,13.005));
#14832=CARTESIAN_POINT('Ctrl Pts',(0.0546129046324092,-17.2546977939649,
13.0038502947236));
#14833=CARTESIAN_POINT('Ctrl Pts',(0.106330167759284,-17.233242056333,12.9996958932764));
#14834=CARTESIAN_POINT('Ctrl Pts',(0.129892073845076,-17.2170927742533,
12.9967480843909));
#14835=CARTESIAN_POINT('Ctrl Pts',(0.157297138725604,-17.1896877093727,
12.9926539494391));
#14836=CARTESIAN_POINT('Ctrl Pts',(0.165594865311311,-17.1798014223953,
12.9912919219764));
#14837=CARTESIAN_POINT('Ctrl Pts',(0.17298843892005,-17.1690588089979,12.99));
#14838=CARTESIAN_POINT('',(-0.21,-17.05,12.99));
#14839=CARTESIAN_POINT('Origin',(0.,-17.05,12.99));
#14840=CARTESIAN_POINT('',(-0.21,-17.05,13.4852272553384));
#14841=CARTESIAN_POINT('',(-0.21,-17.05,12.99));
#14842=CARTESIAN_POINT('',(0.21,-17.05,13.4852272553384));
#14843=CARTESIAN_POINT('Ctrl Pts',(0.21,-17.05,13.4852272553384));
#14844=CARTESIAN_POINT('Ctrl Pts',(0.21,-17.0764055269245,13.4852272553384));
#14845=CARTESIAN_POINT('Ctrl Pts',(0.204715737269596,-17.1045470740907,
13.4860041595441));
#14846=CARTESIAN_POINT('Ctrl Pts',(0.183273763036332,-17.1562762689051,
13.4888007328232));
#14847=CARTESIAN_POINT('Ctrl Pts',(0.167117923970393,-17.179866924128,13.4907789715758));
#14848=CARTESIAN_POINT('Ctrl Pts',(0.129867169887369,-17.217117678211,13.4944848114133));
#14849=CARTESIAN_POINT('Ctrl Pts',(0.106276408305765,-17.2332737100014,
13.4964545565713));
#14850=CARTESIAN_POINT('Ctrl Pts',(0.0545468514058993,-17.2547158248262,
13.4992316551565));
#14851=CARTESIAN_POINT('Ctrl Pts',(0.0264051785092816,-17.26,13.5));
#14852=CARTESIAN_POINT('Ctrl Pts',(-0.0264051785092815,-17.26,13.5));
#14853=CARTESIAN_POINT('Ctrl Pts',(-0.0545468514058992,-17.2547158248262,
13.4992316551565));
#14854=CARTESIAN_POINT('Ctrl Pts',(-0.106276408305765,-17.2332737100014,
13.4964545565713));
#14855=CARTESIAN_POINT('Ctrl Pts',(-0.129867169887368,-17.217117678211,
13.4944848114133));
#14856=CARTESIAN_POINT('Ctrl Pts',(-0.167117923970393,-17.179866924128,
13.4907789715758));
#14857=CARTESIAN_POINT('Ctrl Pts',(-0.183273763036332,-17.1562762689051,
13.4888007328232));
#14858=CARTESIAN_POINT('Ctrl Pts',(-0.204715737269596,-17.1045470740907,
13.4860041595441));
#14859=CARTESIAN_POINT('Ctrl Pts',(-0.21,-17.0764055269245,13.4852272553384));
#14860=CARTESIAN_POINT('Ctrl Pts',(-0.21,-17.05,13.4852272553384));
#14861=CARTESIAN_POINT('Ctrl Pts',(-0.21,-17.05,13.4852272553384));
#14862=CARTESIAN_POINT('Ctrl Pts',(-0.21,-17.0235944730756,13.4852272553384));
#14863=CARTESIAN_POINT('Ctrl Pts',(-0.204715737269596,-16.9954529259093,
13.4860041595441));
#14864=CARTESIAN_POINT('Ctrl Pts',(-0.183273763036332,-16.9437237310949,
13.4888007328232));
#14865=CARTESIAN_POINT('Ctrl Pts',(-0.167117923970393,-16.920133075872,
13.4907789715758));
#14866=CARTESIAN_POINT('Ctrl Pts',(-0.129867169887369,-16.882882321789,
13.4944848114133));
#14867=CARTESIAN_POINT('Ctrl Pts',(-0.106276408305765,-16.8667262899986,
13.4964545565713));
#14868=CARTESIAN_POINT('Ctrl Pts',(-0.0545468514058993,-16.8452841751738,
13.4992316551565));
#14869=CARTESIAN_POINT('Ctrl Pts',(-0.0264051785092816,-16.84,13.5));
#14870=CARTESIAN_POINT('Ctrl Pts',(0.0264051785092815,-16.84,13.5));
#14871=CARTESIAN_POINT('Ctrl Pts',(0.0545468514058992,-16.8452841751738,
13.4992316551565));
#14872=CARTESIAN_POINT('Ctrl Pts',(0.106276408305765,-16.8667262899986,
13.4964545565713));
#14873=CARTESIAN_POINT('Ctrl Pts',(0.129867169887368,-16.882882321789,13.4944848114133));
#14874=CARTESIAN_POINT('Ctrl Pts',(0.167117923970393,-16.920133075872,13.4907789715758));
#14875=CARTESIAN_POINT('Ctrl Pts',(0.183273763036332,-16.9437237310949,
13.4888007328232));
#14876=CARTESIAN_POINT('Ctrl Pts',(0.204715737269596,-16.9954529259093,
13.4860041595441));
#14877=CARTESIAN_POINT('Ctrl Pts',(0.21,-17.0235944730756,13.4852272553384));
#14878=CARTESIAN_POINT('Ctrl Pts',(0.21,-17.05,13.4852272553384));
#14879=CARTESIAN_POINT('',(-0.172988438920051,-16.9309411910021,12.99));
#14880=CARTESIAN_POINT('Origin',(0.,-17.05,12.99));
#14881=CARTESIAN_POINT('Ctrl Pts',(0.17298843892005,-16.9309411910021,12.99));
#14882=CARTESIAN_POINT('Ctrl Pts',(0.165594865311311,-16.9201985776047,
12.9912919219764));
#14883=CARTESIAN_POINT('Ctrl Pts',(0.157297138725604,-16.9103122906273,
12.992653949439));
#14884=CARTESIAN_POINT('Ctrl Pts',(0.129892073845076,-16.8829072257467,
12.9967480843909));
#14885=CARTESIAN_POINT('Ctrl Pts',(0.106330167759284,-16.8667579436671,
12.9996958932764));
#14886=CARTESIAN_POINT('Ctrl Pts',(0.0546129046324093,-16.8453022060351,
13.0038502947236));
#14887=CARTESIAN_POINT('Ctrl Pts',(0.0264512308298517,-16.84,13.005));
#14888=CARTESIAN_POINT('Ctrl Pts',(-0.0264512308298517,-16.84,13.005));
#14889=CARTESIAN_POINT('Ctrl Pts',(-0.054612904632409,-16.8453022060351,
13.0038502947236));
#14890=CARTESIAN_POINT('Ctrl Pts',(-0.106330167759284,-16.8667579436671,
12.9996958932764));
#14891=CARTESIAN_POINT('Ctrl Pts',(-0.129892073845076,-16.8829072257467,
12.9967480843909));
#14892=CARTESIAN_POINT('Ctrl Pts',(-0.157297138725604,-16.9103122906273,
12.9926539494391));
#14893=CARTESIAN_POINT('Ctrl Pts',(-0.165594865311311,-16.9201985776047,
12.9912919219764));
#14894=CARTESIAN_POINT('Ctrl Pts',(-0.17298843892005,-16.9309411910021,
12.99));
#14895=CARTESIAN_POINT('Origin',(0.,-17.05,12.99));
#14896=CARTESIAN_POINT('',(-0.172988438920051,-17.45,12.99));
#14897=CARTESIAN_POINT('Origin',(0.,-17.45,12.));
#14898=CARTESIAN_POINT('',(-1.005,-16.65,12.));
#14899=CARTESIAN_POINT('Origin',(0.,-16.65,12.));
#14900=CARTESIAN_POINT('',(-1.005,-17.45,12.));
#14901=CARTESIAN_POINT('',(-1.005,-17.45,12.));
#14902=CARTESIAN_POINT('Origin',(0.,-17.45,12.));
#14903=CARTESIAN_POINT('Origin',(0.,-17.45,12.));
#14904=CARTESIAN_POINT('',(-1.5,-16.65,12.));
#14905=CARTESIAN_POINT('Origin',(0.,-16.65,12.));
#14906=CARTESIAN_POINT('',(-1.5,-17.45,12.));
#14907=CARTESIAN_POINT('',(-1.5,-17.45,12.));
#14908=CARTESIAN_POINT('Origin',(0.,-17.45,12.));
#14909=CARTESIAN_POINT('Origin',(0.,-16.65,12.));
#14910=CARTESIAN_POINT('Origin',(0.,-17.45,12.));
#14911=CARTESIAN_POINT('',(0.,0.,0.));
#14912=CARTESIAN_POINT('Origin',(0.,-4.15,12.99));
#14913=CARTESIAN_POINT('',(0.172988438920051,-4.26905880899792,12.99));
#14914=CARTESIAN_POINT('',(0.172988438920051,-4.03094119100208,12.99));
#14915=CARTESIAN_POINT('',(0.172988438920051,-4.55,12.99));
#14916=CARTESIAN_POINT('Origin',(0.,-4.15,12.99));
#14917=CARTESIAN_POINT('Origin',(0.,-4.15,12.99));
#14918=CARTESIAN_POINT('',(-0.172988438920051,-4.26905880899792,12.99));
#14919=CARTESIAN_POINT('Ctrl Pts',(-0.172988438920051,-4.26905880899792,
12.99));
#14920=CARTESIAN_POINT('Ctrl Pts',(-0.16559486531131,-4.2798014223953,12.9912919219764));
#14921=CARTESIAN_POINT('Ctrl Pts',(-0.157297138725605,-4.28968770937275,
12.9926539494391));
#14922=CARTESIAN_POINT('Ctrl Pts',(-0.129892073845076,-4.31709277425327,
12.9967480843909));
#14923=CARTESIAN_POINT('Ctrl Pts',(-0.106330167759284,-4.33324205633295,
12.9996958932764));
#14924=CARTESIAN_POINT('Ctrl Pts',(-0.05461290463241,-4.35469779396491,
13.0038502947236));
#14925=CARTESIAN_POINT('Ctrl Pts',(-0.0264512308298516,-4.36,13.005));
#14926=CARTESIAN_POINT('Ctrl Pts',(0.0264512308298515,-4.36,13.005));
#14927=CARTESIAN_POINT('Ctrl Pts',(0.0546129046324099,-4.35469779396491,
13.0038502947236));
#14928=CARTESIAN_POINT('Ctrl Pts',(0.106330167759284,-4.33324205633295,
12.9996958932764));
#14929=CARTESIAN_POINT('Ctrl Pts',(0.129892073845076,-4.31709277425327,
12.9967480843909));
#14930=CARTESIAN_POINT('Ctrl Pts',(0.157297138725605,-4.28968770937275,
12.992653949439));
#14931=CARTESIAN_POINT('Ctrl Pts',(0.165594865311311,-4.2798014223953,12.9912919219764));
#14932=CARTESIAN_POINT('Ctrl Pts',(0.172988438920051,-4.26905880899792,
12.99));
#14933=CARTESIAN_POINT('',(-0.21,-4.15,12.99));
#14934=CARTESIAN_POINT('Origin',(0.,-4.15,12.99));
#14935=CARTESIAN_POINT('',(-0.21,-4.15,13.4852272553384));
#14936=CARTESIAN_POINT('',(-0.21,-4.15,12.99));
#14937=CARTESIAN_POINT('',(0.21,-4.15,13.4852272553384));
#14938=CARTESIAN_POINT('Ctrl Pts',(0.21,-4.15,13.4852272553384));
#14939=CARTESIAN_POINT('Ctrl Pts',(0.21,-4.17640552692446,13.4852272553384));
#14940=CARTESIAN_POINT('Ctrl Pts',(0.204715737269596,-4.20454707409071,
13.4860041595441));
#14941=CARTESIAN_POINT('Ctrl Pts',(0.183273763036332,-4.25627626890513,
13.4888007328232));
#14942=CARTESIAN_POINT('Ctrl Pts',(0.167117923970394,-4.27986692412796,
13.4907789715758));
#14943=CARTESIAN_POINT('Ctrl Pts',(0.129867169887369,-4.31711767821098,
13.4944848114133));
#14944=CARTESIAN_POINT('Ctrl Pts',(0.106276408305765,-4.33327371000135,
13.4964545565713));
#14945=CARTESIAN_POINT('Ctrl Pts',(0.0545468514059003,-4.35471582482622,
13.4992316551565));
#14946=CARTESIAN_POINT('Ctrl Pts',(0.0264051785092814,-4.36,13.5));
#14947=CARTESIAN_POINT('Ctrl Pts',(-0.0264051785092814,-4.36,13.5));
#14948=CARTESIAN_POINT('Ctrl Pts',(-0.0545468514059002,-4.35471582482622,
13.4992316551565));
#14949=CARTESIAN_POINT('Ctrl Pts',(-0.106276408305765,-4.33327371000135,
13.4964545565713));
#14950=CARTESIAN_POINT('Ctrl Pts',(-0.129867169887369,-4.31711767821098,
13.4944848114133));
#14951=CARTESIAN_POINT('Ctrl Pts',(-0.167117923970394,-4.27986692412796,
13.4907789715758));
#14952=CARTESIAN_POINT('Ctrl Pts',(-0.183273763036332,-4.25627626890513,
13.4888007328232));
#14953=CARTESIAN_POINT('Ctrl Pts',(-0.204715737269596,-4.20454707409071,
13.4860041595441));
#14954=CARTESIAN_POINT('Ctrl Pts',(-0.21,-4.17640552692446,13.4852272553384));
#14955=CARTESIAN_POINT('Ctrl Pts',(-0.21,-4.15,13.4852272553384));
#14956=CARTESIAN_POINT('Ctrl Pts',(-0.21,-4.15,13.4852272553384));
#14957=CARTESIAN_POINT('Ctrl Pts',(-0.21,-4.12359447307555,13.4852272553384));
#14958=CARTESIAN_POINT('Ctrl Pts',(-0.204715737269596,-4.09545292590929,
13.4860041595441));
#14959=CARTESIAN_POINT('Ctrl Pts',(-0.183273763036332,-4.04372373109487,
13.4888007328232));
#14960=CARTESIAN_POINT('Ctrl Pts',(-0.167117923970394,-4.02013307587204,
13.4907789715758));
#14961=CARTESIAN_POINT('Ctrl Pts',(-0.129867169887369,-3.98288232178902,
13.4944848114133));
#14962=CARTESIAN_POINT('Ctrl Pts',(-0.106276408305765,-3.96672628999865,
13.4964545565713));
#14963=CARTESIAN_POINT('Ctrl Pts',(-0.0545468514059,-3.94528417517378,13.4992316551565));
#14964=CARTESIAN_POINT('Ctrl Pts',(-0.0264051785092814,-3.94,13.5));
#14965=CARTESIAN_POINT('Ctrl Pts',(0.0264051785092813,-3.94,13.5));
#14966=CARTESIAN_POINT('Ctrl Pts',(0.0545468514058999,-3.94528417517378,
13.4992316551565));
#14967=CARTESIAN_POINT('Ctrl Pts',(0.106276408305765,-3.96672628999865,
13.4964545565713));
#14968=CARTESIAN_POINT('Ctrl Pts',(0.129867169887369,-3.98288232178902,
13.4944848114133));
#14969=CARTESIAN_POINT('Ctrl Pts',(0.167117923970394,-4.02013307587204,
13.4907789715758));
#14970=CARTESIAN_POINT('Ctrl Pts',(0.183273763036331,-4.04372373109487,
13.4888007328232));
#14971=CARTESIAN_POINT('Ctrl Pts',(0.204715737269596,-4.09545292590929,
13.4860041595441));
#14972=CARTESIAN_POINT('Ctrl Pts',(0.21,-4.12359447307555,13.4852272553384));
#14973=CARTESIAN_POINT('Ctrl Pts',(0.21,-4.15,13.4852272553384));
#14974=CARTESIAN_POINT('',(-0.172988438920051,-4.03094119100208,12.99));
#14975=CARTESIAN_POINT('Origin',(0.,-4.15,12.99));
#14976=CARTESIAN_POINT('Ctrl Pts',(0.172988438920051,-4.03094119100208,
12.99));
#14977=CARTESIAN_POINT('Ctrl Pts',(0.165594865311311,-4.0201985776047,12.9912919219764));
#14978=CARTESIAN_POINT('Ctrl Pts',(0.157297138725604,-4.01031229062725,
12.9926539494391));
#14979=CARTESIAN_POINT('Ctrl Pts',(0.129892073845076,-3.98290722574673,
12.9967480843909));
#14980=CARTESIAN_POINT('Ctrl Pts',(0.106330167759284,-3.96675794366705,
12.9996958932764));
#14981=CARTESIAN_POINT('Ctrl Pts',(0.0546129046324106,-3.94530220603509,
13.0038502947236));
#14982=CARTESIAN_POINT('Ctrl Pts',(0.0264512308298516,-3.94,13.005));
#14983=CARTESIAN_POINT('Ctrl Pts',(-0.0264512308298516,-3.94,13.005));
#14984=CARTESIAN_POINT('Ctrl Pts',(-0.0546129046324106,-3.94530220603509,
13.0038502947236));
#14985=CARTESIAN_POINT('Ctrl Pts',(-0.106330167759284,-3.96675794366705,
12.9996958932764));
#14986=CARTESIAN_POINT('Ctrl Pts',(-0.129892073845076,-3.98290722574673,
12.9967480843909));
#14987=CARTESIAN_POINT('Ctrl Pts',(-0.157297138725604,-4.01031229062725,
12.992653949439));
#14988=CARTESIAN_POINT('Ctrl Pts',(-0.165594865311311,-4.0201985776047,
12.9912919219764));
#14989=CARTESIAN_POINT('Ctrl Pts',(-0.172988438920051,-4.03094119100208,
12.99));
#14990=CARTESIAN_POINT('Origin',(0.,-4.15,12.99));
#14991=CARTESIAN_POINT('',(-0.172988438920051,-4.55,12.99));
#14992=CARTESIAN_POINT('Origin',(0.,-4.55,12.));
#14993=CARTESIAN_POINT('',(-1.005,-3.75,12.));
#14994=CARTESIAN_POINT('Origin',(0.,-3.75,12.));
#14995=CARTESIAN_POINT('',(-1.005,-4.55,12.));
#14996=CARTESIAN_POINT('',(-1.005,-4.55,12.));
#14997=CARTESIAN_POINT('Origin',(0.,-4.55,12.));
#14998=CARTESIAN_POINT('Origin',(0.,-4.55,12.));
#14999=CARTESIAN_POINT('',(-1.5,-3.75,12.));
#15000=CARTESIAN_POINT('Origin',(0.,-3.75,12.));
#15001=CARTESIAN_POINT('',(-1.5,-4.55,12.));
#15002=CARTESIAN_POINT('',(-1.5,-4.55,12.));
#15003=CARTESIAN_POINT('Origin',(0.,-4.55,12.));
#15004=CARTESIAN_POINT('Origin',(0.,-3.75,12.));
#15005=CARTESIAN_POINT('Origin',(0.,-4.55,12.));
#15006=CARTESIAN_POINT('',(0.,0.,0.));
#15007=CARTESIAN_POINT('Origin',(0.,-16.65,12.));
#15008=CARTESIAN_POINT('',(-1.005,-15.85,12.));
#15009=CARTESIAN_POINT('Origin',(0.,-15.85,12.));
#15010=CARTESIAN_POINT('',(-1.005,-16.65,12.));
#15011=CARTESIAN_POINT('',(-1.005,-16.65,12.));
#15012=CARTESIAN_POINT('Origin',(0.,-16.65,12.));
#15013=CARTESIAN_POINT('Origin',(0.,-16.65,12.));
#15014=CARTESIAN_POINT('',(-1.3,-15.85,12.));
#15015=CARTESIAN_POINT('Origin',(0.,-15.85,12.));
#15016=CARTESIAN_POINT('',(-1.3,-16.65,12.));
#15017=CARTESIAN_POINT('',(-1.3,-16.65,12.));
#15018=CARTESIAN_POINT('Origin',(0.,-16.65,12.));
#15019=CARTESIAN_POINT('Origin',(0.,-15.85,12.));
#15020=CARTESIAN_POINT('Origin',(0.,-16.65,12.));
#15021=CARTESIAN_POINT('',(0.,0.,0.));
#15022=CARTESIAN_POINT('Origin',(1.,0.9,12.));
#15023=CARTESIAN_POINT('',(0.9422,0.9,12.3350509811954));
#15024=CARTESIAN_POINT('',(0.9422,0.9,11.6649490188046));
#15025=CARTESIAN_POINT('Origin',(0.,0.9,12.));
#15026=CARTESIAN_POINT('Origin',(1.,0.9,12.));
#15027=CARTESIAN_POINT('Origin',(1.,0.9,12.));
#15028=CARTESIAN_POINT('',(0.9422,1.,12.3350509811954));
#15029=CARTESIAN_POINT('',(0.9422,0.9,12.3350509811954));
#15030=CARTESIAN_POINT('',(0.66,1.,12.));
#15031=CARTESIAN_POINT('Origin',(1.,1.,12.));
#15032=CARTESIAN_POINT('',(0.66,2.,12.));
#15033=CARTESIAN_POINT('',(0.66,0.9,12.));
#15034=CARTESIAN_POINT('Origin',(1.,2.,12.));
#15035=CARTESIAN_POINT('',(0.9422,1.,11.6649490188046));
#15036=CARTESIAN_POINT('Origin',(1.,1.,12.));
#15037=CARTESIAN_POINT('',(0.9422,0.9,11.6649490188046));
#15038=CARTESIAN_POINT('Origin',(0.,-1.5,12.));
#15039=CARTESIAN_POINT('',(0.3,1.,11.0460607985831));
#15040=CARTESIAN_POINT('Origin',(0.,1.,12.));
#15041=CARTESIAN_POINT('',(0.3,-1.5,11.0460607985831));
#15042=CARTESIAN_POINT('',(0.3,-1.5,11.0460607985831));
#15043=CARTESIAN_POINT('',(0.0640312423743287,-1.5,12.9979478944314));
#15044=CARTESIAN_POINT('Origin',(0.,-1.5,12.));
#15045=CARTESIAN_POINT('',(0.141067359796645,-1.45556349186105,12.99));
#15046=CARTESIAN_POINT('Ctrl Pts',(0.0640312423743286,-1.5,12.9979478944314));
#15047=CARTESIAN_POINT('Ctrl Pts',(0.069586383475953,-1.49822148706849,
12.9975914604048));
#15048=CARTESIAN_POINT('Ctrl Pts',(0.0750776578932034,-1.49620769804413,
12.9971923790166));
#15049=CARTESIAN_POINT('Ctrl Pts',(0.102998643109694,-1.48462404333102,
12.9949381930495));
#15050=CARTESIAN_POINT('Ctrl Pts',(0.123818356698215,-1.4712051523632,12.9924578498245));
#15051=CARTESIAN_POINT('Ctrl Pts',(0.141067359796645,-1.45556349186105,
12.99));
#15052=CARTESIAN_POINT('',(0.141067359796645,-1.14443650813895,12.99));
#15053=CARTESIAN_POINT('',(0.141067359796645,-1.5,12.99));
#15054=CARTESIAN_POINT('',(-0.141067359796645,-1.14443650813895,12.99));
#15055=CARTESIAN_POINT('Ctrl Pts',(0.141067359796645,-1.14443650813895,
12.99));
#15056=CARTESIAN_POINT('Ctrl Pts',(0.123818356698214,-1.1287948476368,12.9924578498245));
#15057=CARTESIAN_POINT('Ctrl Pts',(0.102998643109694,-1.11537595666898,
12.9949381930495));
#15058=CARTESIAN_POINT('Ctrl Pts',(0.054614114398353,-1.09530253627557,
12.9988444923724));
#15059=CARTESIAN_POINT('Ctrl Pts',(0.0264520736824499,-1.09,13.));
#15060=CARTESIAN_POINT('Ctrl Pts',(-0.0264520736824498,-1.09,13.));
#15061=CARTESIAN_POINT('Ctrl Pts',(-0.0546141143983528,-1.09530253627557,
12.9988444923724));
#15062=CARTESIAN_POINT('Ctrl Pts',(-0.102998643109694,-1.11537595666898,
12.9949381930495));
#15063=CARTESIAN_POINT('Ctrl Pts',(-0.123818356698214,-1.1287948476368,
12.9924578498245));
#15064=CARTESIAN_POINT('Ctrl Pts',(-0.141067359796645,-1.14443650813895,
12.99));
#15065=CARTESIAN_POINT('',(-0.141067359796645,-1.45556349186105,12.99));
#15066=CARTESIAN_POINT('',(-0.141067359796645,-1.5,12.99));
#15067=CARTESIAN_POINT('',(-0.0640312423743287,-1.5,12.9979478944314));
#15068=CARTESIAN_POINT('Ctrl Pts',(-0.141067359796645,-1.45556349186105,
12.99));
#15069=CARTESIAN_POINT('Ctrl Pts',(-0.123818356698214,-1.4712051523632,
12.9924578498245));
#15070=CARTESIAN_POINT('Ctrl Pts',(-0.102998643109694,-1.48462404333102,
12.9949381930495));
#15071=CARTESIAN_POINT('Ctrl Pts',(-0.0750776578932035,-1.49620769804413,
12.9971923790166));
#15072=CARTESIAN_POINT('Ctrl Pts',(-0.0695863834759529,-1.49822148706849,
12.9975914604048));
#15073=CARTESIAN_POINT('Ctrl Pts',(-0.0640312423743286,-1.5,12.9979478944314));
#15074=CARTESIAN_POINT('',(-0.3,-1.5,11.0460607985831));
#15075=CARTESIAN_POINT('Origin',(0.,-1.5,12.));
#15076=CARTESIAN_POINT('',(-0.3,1.,11.0460607985831));
#15077=CARTESIAN_POINT('',(-0.3,-1.5,11.0460607985831));
#15078=CARTESIAN_POINT('Origin',(0.,1.,12.));
#15079=CARTESIAN_POINT('Origin',(0.,1.,12.));
#15080=CARTESIAN_POINT('',(-0.3,1.,10.72));
#15081=CARTESIAN_POINT('',(-0.3,1.,11.36));
#15082=CARTESIAN_POINT('',(0.3,1.,10.72));
#15083=CARTESIAN_POINT('',(0.15,1.,10.72));
#15084=CARTESIAN_POINT('',(0.3,1.,12.));
#15085=CARTESIAN_POINT('Origin',(0.,2.,12.));
#15086=CARTESIAN_POINT('',(-4.,2.,12.));
#15087=CARTESIAN_POINT('Origin',(0.,2.,12.));
#15088=CARTESIAN_POINT('Origin',(0.3,-1.6,10.72));
#15089=CARTESIAN_POINT('',(-0.3,-1.5,10.72));
#15090=CARTESIAN_POINT('',(-0.3,-1.6,10.72));
#15091=CARTESIAN_POINT('',(0.3,-1.5,10.72));
#15092=CARTESIAN_POINT('',(0.15,-1.5,10.72));
#15093=CARTESIAN_POINT('',(0.3,-1.6,10.72));
#15094=CARTESIAN_POINT('Origin',(-0.3,-1.6,10.72));
#15095=CARTESIAN_POINT('',(-0.3,-1.5,11.36));
#15096=CARTESIAN_POINT('Origin',(0.,-1.3,12.99));
#15097=CARTESIAN_POINT('Origin',(0.,-1.3,12.99));
#15098=CARTESIAN_POINT('Origin',(0.,-1.3,12.99));
#15099=CARTESIAN_POINT('Origin',(0.,-1.3,12.99));
#15100=CARTESIAN_POINT('',(0.0640312423743287,-1.5,13.5987182365883));
#15101=CARTESIAN_POINT('',(0.0640312423743287,-1.5,12.99));
#15102=CARTESIAN_POINT('',(-0.0640312423743287,-1.5,13.5987182365883));
#15103=CARTESIAN_POINT('Ctrl Pts',(-0.0640312423743288,-1.5,13.5987182365883));
#15104=CARTESIAN_POINT('Ctrl Pts',(-0.0695623721690264,-1.49822917443756,
13.5984967059243));
#15105=CARTESIAN_POINT('Ctrl Pts',(-0.0750312749053374,-1.49622475645458,
13.5982488123351));
#15106=CARTESIAN_POINT('Ctrl Pts',(-0.106271159541076,-1.48327680083123,
13.5966769093301));
#15107=CARTESIAN_POINT('Ctrl Pts',(-0.129864750292352,-1.467120097806,13.5948307595328));
#15108=CARTESIAN_POINT('Ctrl Pts',(-0.167120287247804,-1.42986456085055,
13.5913581688701));
#15109=CARTESIAN_POINT('Ctrl Pts',(-0.183276841782292,-1.4062710523005,
13.5895050296478));
#15110=CARTESIAN_POINT('Ctrl Pts',(-0.20471752266132,-1.35454055536511,
13.586886062954));
#15111=CARTESIAN_POINT('Ctrl Pts',(-0.21,-1.32640093420375,13.5861588823318));
#15112=CARTESIAN_POINT('Ctrl Pts',(-0.21,-1.27359906579625,13.5861588823318));
#15113=CARTESIAN_POINT('Ctrl Pts',(-0.20471752266132,-1.24545944463489,
13.586886062954));
#15114=CARTESIAN_POINT('Ctrl Pts',(-0.183276841782292,-1.1937289476995,
13.5895050296478));
#15115=CARTESIAN_POINT('Ctrl Pts',(-0.167120287247804,-1.17013543914945,
13.5913581688701));
#15116=CARTESIAN_POINT('Ctrl Pts',(-0.129864750292352,-1.132879902194,13.5948307595328));
#15117=CARTESIAN_POINT('Ctrl Pts',(-0.106271159541076,-1.11672319916877,
13.5966769093301));
#15118=CARTESIAN_POINT('Ctrl Pts',(-0.0545403836274686,-1.0952824096556,
13.5992798562698));
#15119=CARTESIAN_POINT('Ctrl Pts',(-0.0264006657112965,-1.09,13.6));
#15120=CARTESIAN_POINT('Ctrl Pts',(0.0264006657112964,-1.09,13.6));
#15121=CARTESIAN_POINT('Ctrl Pts',(0.0545403836274687,-1.0952824096556,
13.5992798562698));
#15122=CARTESIAN_POINT('Ctrl Pts',(0.106271159541076,-1.11672319916877,
13.5966769093301));
#15123=CARTESIAN_POINT('Ctrl Pts',(0.129864750292352,-1.132879902194,13.5948307595328));
#15124=CARTESIAN_POINT('Ctrl Pts',(0.167120287247804,-1.17013543914945,
13.5913581688701));
#15125=CARTESIAN_POINT('Ctrl Pts',(0.183276841782292,-1.1937289476995,13.5895050296478));
#15126=CARTESIAN_POINT('Ctrl Pts',(0.20471752266132,-1.24545944463489,13.586886062954));
#15127=CARTESIAN_POINT('Ctrl Pts',(0.21,-1.27359906579625,13.5861588823318));
#15128=CARTESIAN_POINT('Ctrl Pts',(0.21,-1.3,13.5861588823318));
#15129=CARTESIAN_POINT('Ctrl Pts',(0.21,-1.32640093420375,13.5861588823318));
#15130=CARTESIAN_POINT('Ctrl Pts',(0.20471752266132,-1.35454055536511,13.586886062954));
#15131=CARTESIAN_POINT('Ctrl Pts',(0.183276841782292,-1.4062710523005,13.5895050296478));
#15132=CARTESIAN_POINT('Ctrl Pts',(0.167120287247804,-1.42986456085055,
13.5913581688701));
#15133=CARTESIAN_POINT('Ctrl Pts',(0.129864750292352,-1.467120097806,13.5948307595328));
#15134=CARTESIAN_POINT('Ctrl Pts',(0.106271159541076,-1.48327680083123,
13.5966769093301));
#15135=CARTESIAN_POINT('Ctrl Pts',(0.0750312749053373,-1.49622475645458,
13.5982488123351));
#15136=CARTESIAN_POINT('Ctrl Pts',(0.0695623721690265,-1.49822917443756,
13.5984967059243));
#15137=CARTESIAN_POINT('Ctrl Pts',(0.0640312423743287,-1.5,13.5987182365883));
#15138=CARTESIAN_POINT('',(-0.0640312423743287,-1.5,12.99));
#15139=CARTESIAN_POINT('Origin',(0.,-1.3,12.99));
#15140=CARTESIAN_POINT('Origin',(0.3,-1.6,12.));
#15141=CARTESIAN_POINT('',(0.3,-1.5,12.));
#15142=CARTESIAN_POINT('Origin',(0.,-1.,12.));
#15143=CARTESIAN_POINT('',(-4.,-1.,12.));
#15144=CARTESIAN_POINT('Origin',(0.,-1.,12.));
#15145=CARTESIAN_POINT('',(-1.6,-1.,12.));
#15146=CARTESIAN_POINT('Origin',(0.,-1.,12.));
#15147=CARTESIAN_POINT('Origin',(0.,-1.,12.));
#15148=CARTESIAN_POINT('',(-4.,-1.,12.));
#15149=CARTESIAN_POINT('Origin',(0.,-1.5,12.));
#15150=CARTESIAN_POINT('',(-1.6,-1.5,12.));
#15151=CARTESIAN_POINT('',(-1.6,-1.5,12.));
#15152=CARTESIAN_POINT('Origin',(0.,-1.5,12.));
#15153=CARTESIAN_POINT('Origin',(0.,-1.5,12.));
#15154=CARTESIAN_POINT('Origin',(0.,-1.5,12.));
#15155=CARTESIAN_POINT('',(0.,0.,0.));
#15156=CARTESIAN_POINT('Origin',(1.,3.7,12.));
#15157=CARTESIAN_POINT('',(0.835,3.7,12.));
#15158=CARTESIAN_POINT('Origin',(1.,3.7,12.));
#15159=CARTESIAN_POINT('',(0.835,4.8,12.));
#15160=CARTESIAN_POINT('',(0.835,3.7,12.));
#15161=CARTESIAN_POINT('Origin',(1.,4.8,12.));
#15162=CARTESIAN_POINT('Origin',(1.,3.7,12.));
#15163=CARTESIAN_POINT('Origin',(1.,2.,12.));
#15164=CARTESIAN_POINT('',(0.5,2.,12.));
#15165=CARTESIAN_POINT('Origin',(1.,2.,12.));
#15166=CARTESIAN_POINT('',(0.6,2.,12.));
#15167=CARTESIAN_POINT('Origin',(1.,2.,12.));
#15168=CARTESIAN_POINT('Origin',(1.,2.,12.));
#15169=CARTESIAN_POINT('',(0.5,4.8,12.));
#15170=CARTESIAN_POINT('Origin',(1.,4.8,12.));
#15171=CARTESIAN_POINT('',(0.5,2.,12.));
#15172=CARTESIAN_POINT('Origin',(1.,4.8,12.));
#15173=CARTESIAN_POINT('Origin',(1.,1.,12.));
#15174=CARTESIAN_POINT('',(0.6,1.,12.));
#15175=CARTESIAN_POINT('',(0.6,1.,12.));
#15176=CARTESIAN_POINT('Origin',(1.,1.,12.));
#15177=CARTESIAN_POINT('Origin',(1.,1.,12.));
#15178=CARTESIAN_POINT('',(0.,0.,0.));
#15179=CARTESIAN_POINT('Origin',(1.,2.,12.));
#15180=CARTESIAN_POINT('',(0.495,3.5,12.));
#15181=CARTESIAN_POINT('Origin',(1.,3.5,12.));
#15182=CARTESIAN_POINT('',(0.495,2.,12.));
#15183=CARTESIAN_POINT('',(0.495,2.,12.));
#15184=CARTESIAN_POINT('Origin',(1.,2.,12.));
#15185=CARTESIAN_POINT('Origin',(1.,2.,12.));
#15186=CARTESIAN_POINT('',(0.3,3.5,12.));
#15187=CARTESIAN_POINT('Origin',(1.,3.5,12.));
#15188=CARTESIAN_POINT('',(0.3,2.,12.));
#15189=CARTESIAN_POINT('',(0.3,2.,12.));
#15190=CARTESIAN_POINT('Origin',(1.,2.,12.));
#15191=CARTESIAN_POINT('Origin',(1.,3.5,12.));
#15192=CARTESIAN_POINT('Origin',(1.,2.,12.));
#15193=CARTESIAN_POINT('',(0.,0.,0.));
#15194=CARTESIAN_POINT('Origin',(1.,4.4,12.));
#15195=CARTESIAN_POINT('',(0.495,4.8,12.));
#15196=CARTESIAN_POINT('Origin',(1.,4.8,12.));
#15197=CARTESIAN_POINT('',(0.495,4.4,12.));
#15198=CARTESIAN_POINT('',(0.495,4.4,12.));
#15199=CARTESIAN_POINT('Origin',(1.,4.4,12.));
#15200=CARTESIAN_POINT('Origin',(1.,4.4,12.));
#15201=CARTESIAN_POINT('',(0.3,4.8,12.));
#15202=CARTESIAN_POINT('Origin',(1.,4.8,12.));
#15203=CARTESIAN_POINT('',(0.3,4.4,12.));
#15204=CARTESIAN_POINT('',(0.3,4.4,12.));
#15205=CARTESIAN_POINT('Origin',(1.,4.4,12.));
#15206=CARTESIAN_POINT('Origin',(1.,4.8,12.));
#15207=CARTESIAN_POINT('Origin',(1.,4.4,12.));
#15208=CARTESIAN_POINT('',(0.,0.,0.));
#15209=CARTESIAN_POINT('Origin',(1.,4.8,12.));
#15210=CARTESIAN_POINT('',(0.775,5.,12.));
#15211=CARTESIAN_POINT('Origin',(1.,5.,12.));
#15212=CARTESIAN_POINT('',(0.775,4.8,12.));
#15213=CARTESIAN_POINT('',(0.775,4.8,12.));
#15214=CARTESIAN_POINT('Origin',(1.,4.8,12.));
#15215=CARTESIAN_POINT('Origin',(1.,4.8,12.));
#15216=CARTESIAN_POINT('',(0.2,5.,12.));
#15217=CARTESIAN_POINT('Origin',(1.,5.,12.));
#15218=CARTESIAN_POINT('',(0.2,4.8,12.));
#15219=CARTESIAN_POINT('',(0.2,4.8,12.));
#15220=CARTESIAN_POINT('Origin',(1.,4.8,12.));
#15221=CARTESIAN_POINT('Origin',(1.,5.,12.));
#15222=CARTESIAN_POINT('Origin',(1.,4.8,12.));
#15223=CARTESIAN_POINT('',(0.,0.,0.));
#15224=CARTESIAN_POINT('Origin',(-1.,0.,0.35));
#15225=CARTESIAN_POINT('',(-1.,-0.26,0.6));
#15226=CARTESIAN_POINT('',(-1.,-0.3,0.56));
#15227=CARTESIAN_POINT('',(-1.,-0.2675,0.5925));
#15228=CARTESIAN_POINT('',(-1.,0.26,0.6));
#15229=CARTESIAN_POINT('',(-1.,0.,0.6));
#15230=CARTESIAN_POINT('',(-1.,0.3,0.56));
#15231=CARTESIAN_POINT('',(-1.,0.2675,0.5925));
#15232=CARTESIAN_POINT('',(-1.,0.3,0.04));
#15233=CARTESIAN_POINT('',(-1.,0.3,0.175));
#15234=CARTESIAN_POINT('',(-1.,0.26,0.));
#15235=CARTESIAN_POINT('',(-1.,0.2925,0.0325));
#15236=CARTESIAN_POINT('',(-1.,-0.26,0.));
#15237=CARTESIAN_POINT('',(-1.,0.,0.));
#15238=CARTESIAN_POINT('',(-1.,-0.3,0.04));
#15239=CARTESIAN_POINT('',(-1.,-0.2925,0.0325));
#15240=CARTESIAN_POINT('',(-1.,-0.3,0.175));
#15241=CARTESIAN_POINT('Origin',(0.75,0.28,0.02));
#15242=CARTESIAN_POINT('',(1.,0.3,0.04));
#15243=CARTESIAN_POINT('',(0.75,0.3,0.04));
#15244=CARTESIAN_POINT('',(1.,0.26,0.));
#15245=CARTESIAN_POINT('',(1.,0.2925,0.0325));
#15246=CARTESIAN_POINT('',(0.75,0.26,0.));
#15247=CARTESIAN_POINT('Origin',(1.5,0.3,0.));
#15248=CARTESIAN_POINT('',(1.,0.3,0.56));
#15249=CARTESIAN_POINT('',(0.75,0.3,0.56));
#15250=CARTESIAN_POINT('',(1.,0.3,0.175));
#15251=CARTESIAN_POINT('Origin',(0.75,0.28,0.58));
#15252=CARTESIAN_POINT('',(1.,0.26,0.6));
#15253=CARTESIAN_POINT('',(0.75,0.26,0.6));
#15254=CARTESIAN_POINT('',(1.,0.2675,0.5925));
#15255=CARTESIAN_POINT('Origin',(0.,0.,0.6));
#15256=CARTESIAN_POINT('',(1.,-0.26,0.6));
#15257=CARTESIAN_POINT('',(-0.75,-0.26,0.6));
#15258=CARTESIAN_POINT('',(1.,0.,0.6));
#15259=CARTESIAN_POINT('Origin',(1.,0.,0.35));
#15260=CARTESIAN_POINT('',(1.,-0.26,0.));
#15261=CARTESIAN_POINT('',(1.,-0.3,0.04));
#15262=CARTESIAN_POINT('',(1.,-0.2925,0.0325));
#15263=CARTESIAN_POINT('',(1.,0.,0.));
#15264=CARTESIAN_POINT('',(1.,-0.3,0.56));
#15265=CARTESIAN_POINT('',(1.,-0.2675,0.5925));
#15266=CARTESIAN_POINT('',(1.,-0.3,0.175));
#15267=CARTESIAN_POINT('Origin',(0.,0.,0.));
#15268=CARTESIAN_POINT('',(-0.75,-0.26,0.));
#15269=CARTESIAN_POINT('Origin',(-0.75,-0.28,0.58));
#15270=CARTESIAN_POINT('',(-0.75,-0.3,0.56));
#15271=CARTESIAN_POINT('Origin',(-0.75,-0.28,0.02));
#15272=CARTESIAN_POINT('',(-0.75,-0.3,0.04));
#15273=CARTESIAN_POINT('Origin',(-1.5,-0.3,0.));
#15274=CARTESIAN_POINT('',(0.,0.,0.));
#15275=CARTESIAN_POINT('Origin',(0.0721687836487032,0.,-0.125));
#15276=CARTESIAN_POINT('',(0.0721687836487032,0.,-0.125));
#15277=CARTESIAN_POINT('',(0.144337567297406,0.,0.));
#15278=CARTESIAN_POINT('',(0.117710979560879,0.,-0.0461186027918559));
#15279=CARTESIAN_POINT('',(0.0721687836487032,-0.25,-0.125));
#15280=CARTESIAN_POINT('',(0.0721687836487032,0.,-0.125));
#15281=CARTESIAN_POINT('',(0.144337567297406,-0.25,0.));
#15282=CARTESIAN_POINT('',(0.144337567297406,-0.25,0.));
#15283=CARTESIAN_POINT('',(0.144337567297406,0.,0.));
#15284=CARTESIAN_POINT('Origin',(-0.0721687836487032,0.,-0.125));
#15285=CARTESIAN_POINT('',(-0.0721687836487032,0.,-0.125));
#15286=CARTESIAN_POINT('',(0.0739156081756484,0.,-0.125));
#15287=CARTESIAN_POINT('',(-0.0721687836487032,-0.25,-0.125));
#15288=CARTESIAN_POINT('',(-0.0721687836487032,0.,-0.125));
#15289=CARTESIAN_POINT('',(0.0721687836487032,-0.25,-0.125));
#15290=CARTESIAN_POINT('Origin',(-0.144337567297406,0.,-4.16333634234434E-17));
#15291=CARTESIAN_POINT('',(-0.144337567297406,0.,-1.76762539787485E-17));
#15292=CARTESIAN_POINT('',(-0.0987953713852306,0.,-0.0788813972081442));
#15293=CARTESIAN_POINT('',(-0.144337567297406,-0.25,-2.77555756156289E-17));
#15294=CARTESIAN_POINT('',(-0.144337567297406,0.,-1.76762539787485E-17));
#15295=CARTESIAN_POINT('',(-0.0721687836487032,-0.25,-0.125));
#15296=CARTESIAN_POINT('Origin',(-0.0721687836487033,0.,0.125));
#15297=CARTESIAN_POINT('',(-0.0721687836487033,0.,0.125));
#15298=CARTESIAN_POINT('',(-0.0627109795608791,0.,0.141381397208144));
#15299=CARTESIAN_POINT('',(-0.0721687836487033,-0.25,0.125));
#15300=CARTESIAN_POINT('',(-0.0721687836487033,0.,0.125));
#15301=CARTESIAN_POINT('',(-0.144337567297406,-0.25,-1.76762539787485E-17));
#15302=CARTESIAN_POINT('Origin',(0.0721687836487032,0.,0.125));
#15303=CARTESIAN_POINT('',(0.0721687836487032,0.,0.125));
#15304=CARTESIAN_POINT('',(0.146084391824352,0.,0.125));
#15305=CARTESIAN_POINT('',(0.0721687836487032,-0.25,0.125));
#15306=CARTESIAN_POINT('',(0.0721687836487032,0.,0.125));
#15307=CARTESIAN_POINT('',(-0.0721687836487033,-0.25,0.125));
#15308=CARTESIAN_POINT('Origin',(0.144337567297406,0.,0.));
#15309=CARTESIAN_POINT('',(0.153795371385231,0.,-0.0163813972081441));
#15310=CARTESIAN_POINT('',(0.0721687836487032,-0.25,0.125));
#15311=CARTESIAN_POINT('Origin',(0.,-0.25,0.));
#15312=CARTESIAN_POINT('Origin',(0.22,0.,0.));
#15313=CARTESIAN_POINT('',(-0.22,-8.67361737988404E-18,-2.69422295812418E-17));
#15314=CARTESIAN_POINT('Origin',(0.,0.,0.));
#15315=CARTESIAN_POINT('Origin',(0.,-0.015,0.));
#15316=CARTESIAN_POINT('',(-0.24505,-0.02505,-3.00099698131059E-17));
#15317=CARTESIAN_POINT('Origin',(0.,-0.02505,0.));
#15318=CARTESIAN_POINT('',(-0.235,-0.015,-2.87791997799628E-17));
#15319=CARTESIAN_POINT('Origin',(0.,-0.3775,0.));
#15320=CARTESIAN_POINT('',(-0.24505,-0.72995,3.00099698131059E-17));
#15321=CARTESIAN_POINT('Origin',(0.,-0.72995,0.));
#15322=CARTESIAN_POINT('',(-0.24505,-0.3775,-3.00099698131059E-17));
#15323=CARTESIAN_POINT('Origin',(0.,-0.7625,0.));
#15324=CARTESIAN_POINT('',(-0.175,-0.8,-2.14313189850787E-17));
#15325=CARTESIAN_POINT('Origin',(0.,-0.8,0.));
#15326=CARTESIAN_POINT('',(-0.2125,-0.7625,-2.60237444818813E-17));
#15327=CARTESIAN_POINT('Origin',(0.,-0.8,0.));
#15328=CARTESIAN_POINT('',(0.,0.,0.));
#15329=CARTESIAN_POINT('',(0.,0.,0.));
#15330=CARTESIAN_POINT('Origin',(1.,3.4,12.));
#15331=CARTESIAN_POINT('',(-0.5,3.5,12.));
#15332=CARTESIAN_POINT('Origin',(1.,3.5,12.));
#15333=CARTESIAN_POINT('',(-0.5,4.4,12.));
#15334=CARTESIAN_POINT('',(-0.5,3.4,12.));
#15335=CARTESIAN_POINT('Origin',(1.,4.4,12.));
#15336=CARTESIAN_POINT('Origin',(11.,3.4,12.));
#15337=CARTESIAN_POINT('',(9.5,3.5,12.));
#15338=CARTESIAN_POINT('Origin',(11.,3.5,12.));
#15339=CARTESIAN_POINT('',(9.5,4.4,12.));
#15340=CARTESIAN_POINT('',(9.5,3.4,12.));
#15341=CARTESIAN_POINT('Origin',(11.,4.4,12.));
#15342=CARTESIAN_POINT('Origin',(11.,3.5,12.));
#15343=CARTESIAN_POINT('',(9.26794919243112,3.5,13.));
#15344=CARTESIAN_POINT('',(9.26794919243112,4.4,13.));
#15345=CARTESIAN_POINT('',(9.26794919243112,3.5,13.));
#15346=CARTESIAN_POINT('',(9.26794919243112,3.5,11.));
#15347=CARTESIAN_POINT('Origin',(11.,3.5,12.));
#15348=CARTESIAN_POINT('',(9.26794919243112,4.4,11.));
#15349=CARTESIAN_POINT('',(9.26794919243112,3.5,11.));
#15350=CARTESIAN_POINT('Origin',(11.,4.4,12.));
#15351=CARTESIAN_POINT('Origin',(6.,4.4,12.));
#15352=CARTESIAN_POINT('',(2.73205080756888,4.4,11.));
#15353=CARTESIAN_POINT('',(1.,4.4,11.));
#15354=CARTESIAN_POINT('',(2.73205080756888,4.4,13.));
#15355=CARTESIAN_POINT('Origin',(1.,4.4,12.));
#15356=CARTESIAN_POINT('',(11.,4.4,13.));
#15357=CARTESIAN_POINT('Origin',(11.,3.5,11.));
#15358=CARTESIAN_POINT('',(2.73205080756888,3.5,11.));
#15359=CARTESIAN_POINT('',(1.,3.5,11.));
#15360=CARTESIAN_POINT('',(2.73205080756888,3.5,11.));
#15361=CARTESIAN_POINT('Origin',(1.,3.5,12.));
#15362=CARTESIAN_POINT('',(2.73205080756888,3.5,13.));
#15363=CARTESIAN_POINT('',(2.73205080756888,3.5,13.));
#15364=CARTESIAN_POINT('Origin',(1.,3.5,12.));
#15365=CARTESIAN_POINT('Origin',(1.,3.5,13.));
#15366=CARTESIAN_POINT('',(11.,3.5,13.));
#15367=CARTESIAN_POINT('Origin',(6.,3.5,12.));
#15368=CARTESIAN_POINT('',(0.,0.,0.));
#15369=CARTESIAN_POINT('Origin',(1.,3.3,12.));
#15370=CARTESIAN_POINT('',(-0.1,3.5,12.));
#15371=CARTESIAN_POINT('Origin',(1.,3.5,12.));
#15372=CARTESIAN_POINT('',(-0.1,3.3,12.));
#15373=CARTESIAN_POINT('',(-0.1,3.3,12.));
#15374=CARTESIAN_POINT('Origin',(1.,3.3,12.));
#15375=CARTESIAN_POINT('Origin',(1.,3.3,12.));
#15376=CARTESIAN_POINT('',(-1.,3.5,12.));
#15377=CARTESIAN_POINT('Origin',(1.,3.5,12.));
#15378=CARTESIAN_POINT('',(-1.,3.3,12.));
#15379=CARTESIAN_POINT('',(-1.,3.3,12.));
#15380=CARTESIAN_POINT('Origin',(1.,3.3,12.));
#15381=CARTESIAN_POINT('Origin',(1.,3.5,12.));
#15382=CARTESIAN_POINT('Origin',(1.,3.3,12.));
#15383=CARTESIAN_POINT('',(0.,0.,0.));
#15384=CARTESIAN_POINT('Origin',(1.,4.4,12.));
#15385=CARTESIAN_POINT('',(-0.1,4.6,12.));
#15386=CARTESIAN_POINT('Origin',(1.,4.6,12.));
#15387=CARTESIAN_POINT('',(-0.1,4.4,12.));
#15388=CARTESIAN_POINT('',(-0.1,4.4,12.));
#15389=CARTESIAN_POINT('Origin',(1.,4.4,12.));
#15390=CARTESIAN_POINT('Origin',(1.,4.4,12.));
#15391=CARTESIAN_POINT('',(-1.,4.6,12.));
#15392=CARTESIAN_POINT('Origin',(1.,4.6,12.));
#15393=CARTESIAN_POINT('',(-1.,4.4,12.));
#15394=CARTESIAN_POINT('',(-1.,4.4,12.));
#15395=CARTESIAN_POINT('Origin',(1.,4.4,12.));
#15396=CARTESIAN_POINT('Origin',(1.,4.6,12.));
#15397=CARTESIAN_POINT('Origin',(1.,4.4,12.));
#15398=CARTESIAN_POINT('',(0.,0.,0.));
#15399=CARTESIAN_POINT('Origin',(11.,3.3,12.));
#15400=CARTESIAN_POINT('',(9.9,3.5,12.));
#15401=CARTESIAN_POINT('Origin',(11.,3.5,12.));
#15402=CARTESIAN_POINT('',(9.9,3.3,12.));
#15403=CARTESIAN_POINT('',(9.9,3.3,12.));
#15404=CARTESIAN_POINT('Origin',(11.,3.3,12.));
#15405=CARTESIAN_POINT('Origin',(11.,3.3,12.));
#15406=CARTESIAN_POINT('',(9.,3.5,12.));
#15407=CARTESIAN_POINT('Origin',(11.,3.5,12.));
#15408=CARTESIAN_POINT('',(9.,3.3,12.));
#15409=CARTESIAN_POINT('',(9.,3.3,12.));
#15410=CARTESIAN_POINT('Origin',(11.,3.3,12.));
#15411=CARTESIAN_POINT('Origin',(11.,3.5,12.));
#15412=CARTESIAN_POINT('Origin',(11.,3.3,12.));
#15413=CARTESIAN_POINT('',(0.,0.,0.));
#15414=CARTESIAN_POINT('Origin',(11.,4.4,12.));
#15415=CARTESIAN_POINT('',(9.9,4.6,12.));
#15416=CARTESIAN_POINT('Origin',(11.,4.6,12.));
#15417=CARTESIAN_POINT('',(9.9,4.4,12.));
#15418=CARTESIAN_POINT('',(9.9,4.4,12.));
#15419=CARTESIAN_POINT('Origin',(11.,4.4,12.));
#15420=CARTESIAN_POINT('Origin',(11.,4.4,12.));
#15421=CARTESIAN_POINT('',(9.,4.6,12.));
#15422=CARTESIAN_POINT('Origin',(11.,4.6,12.));
#15423=CARTESIAN_POINT('',(9.,4.4,12.));
#15424=CARTESIAN_POINT('',(9.,4.4,12.));
#15425=CARTESIAN_POINT('Origin',(11.,4.4,12.));
#15426=CARTESIAN_POINT('Origin',(11.,4.6,12.));
#15427=CARTESIAN_POINT('Origin',(11.,4.4,12.));
#15428=CARTESIAN_POINT('',(0.,0.,0.));
#15429=CARTESIAN_POINT('',(0.,0.,0.));
#15430=CARTESIAN_POINT('Origin',(0.,0.,0.));
#15431=CARTESIAN_POINT('',(-0.976185,-0.246528389340863,-1.19548183562566E-16));
#15432=CARTESIAN_POINT('',(-1.19548183562566E-16,-0.246528389340863,0.976185));
#15433=CARTESIAN_POINT('Origin',(0.,-0.246528389340863,0.));
#15434=CARTESIAN_POINT('Origin',(0.,-0.246528389340863,0.));
#15435=CARTESIAN_POINT('',(-1.19548183562566E-16,0.246528389340863,0.976185));
#15436=CARTESIAN_POINT('Origin',(-1.22464679914735E-16,0.,1.));
#15437=CARTESIAN_POINT('',(-0.976185,0.246528389340863,1.19548183562566E-16));
#15438=CARTESIAN_POINT('Origin',(0.,0.246528389340863,0.));
#15439=CARTESIAN_POINT('Origin',(0.,0.246528389340863,0.));
#15440=CARTESIAN_POINT('Origin',(0.,0.,0.));
#15441=CARTESIAN_POINT('',(-0.976185,0.45,-1.19548183562566E-16));
#15442=CARTESIAN_POINT('',(-0.976185,0.,-1.19548183562566E-16));
#15443=CARTESIAN_POINT('Origin',(0.,0.45,0.));
#15444=CARTESIAN_POINT('Origin',(0.,0.,0.));
#15445=CARTESIAN_POINT('',(-0.5,-0.39,-6.12323399573677E-17));
#15446=CARTESIAN_POINT('Origin',(0.,-0.39,0.));
#15447=CARTESIAN_POINT('',(-0.5,0.39,-6.12323399573677E-17));
#15448=CARTESIAN_POINT('',(-0.5,0.,-6.12323399573677E-17));
#15449=CARTESIAN_POINT('Origin',(0.,0.39,0.));
#15450=CARTESIAN_POINT('Origin',(0.,0.42,0.));
#15451=CARTESIAN_POINT('',(-0.56,0.45,-6.85802207522518E-17));
#15452=CARTESIAN_POINT('',(-0.53,0.42,-6.49062803548097E-17));
#15453=CARTESIAN_POINT('Origin',(0.,0.45,0.));
#15454=CARTESIAN_POINT('Origin',(0.976185,0.45,0.));
#15455=CARTESIAN_POINT('Origin',(0.,0.,0.));
#15456=CARTESIAN_POINT('',(-0.976185,-0.45,-1.19548183562566E-16));
#15457=CARTESIAN_POINT('Origin',(0.,-0.45,0.));
#15458=CARTESIAN_POINT('',(-0.976185,0.,-1.19548183562566E-16));
#15459=CARTESIAN_POINT('Origin',(0.56,-0.45,0.));
#15460=CARTESIAN_POINT('',(-0.56,-0.45,-6.85802207522518E-17));
#15461=CARTESIAN_POINT('Origin',(0.,-0.45,0.));
#15462=CARTESIAN_POINT('Origin',(0.,-0.42,0.));
#15463=CARTESIAN_POINT('',(-0.53,-0.42,-6.49062803548097E-17));
#15464=CARTESIAN_POINT('',(0.,0.,0.));
#15465=CARTESIAN_POINT('Origin',(0.,0.,0.));
#15466=CARTESIAN_POINT('',(-1.023815,0.246528389340863,-1.25381176266905E-16));
#15467=CARTESIAN_POINT('',(-1.25381176266905E-16,0.246528389340863,1.023815));
#15468=CARTESIAN_POINT('Origin',(0.,0.246528389340863,0.));
#15469=CARTESIAN_POINT('Origin',(0.,0.246528389340863,0.));
#15470=CARTESIAN_POINT('',(-1.25381176266905E-16,-0.246528389340863,1.023815));
#15471=CARTESIAN_POINT('Origin',(-1.22464679914735E-16,0.,1.));
#15472=CARTESIAN_POINT('',(-1.023815,-0.246528389340863,1.25381176266905E-16));
#15473=CARTESIAN_POINT('Origin',(0.,-0.246528389340863,0.));
#15474=CARTESIAN_POINT('Origin',(0.,-0.246528389340863,0.));
#15475=CARTESIAN_POINT('Origin',(0.,0.,0.));
#15476=CARTESIAN_POINT('',(-1.023815,-0.45,-1.25381176266905E-16));
#15477=CARTESIAN_POINT('Origin',(0.,-0.45,0.));
#15478=CARTESIAN_POINT('',(-1.023815,0.,-1.25381176266905E-16));
#15479=CARTESIAN_POINT('Origin',(1.44,0.45,0.));
#15480=CARTESIAN_POINT('',(-1.44,0.45,-1.76349139077219E-16));
#15481=CARTESIAN_POINT('Origin',(0.,0.45,0.));
#15482=CARTESIAN_POINT('',(-1.023815,0.45,-1.25381176266905E-16));
#15483=CARTESIAN_POINT('Origin',(0.,0.45,0.));
#15484=CARTESIAN_POINT('Origin',(0.,0.42,0.));
#15485=CARTESIAN_POINT('',(-1.5,0.39,-1.83697019872103E-16));
#15486=CARTESIAN_POINT('Origin',(0.,0.39,0.));
#15487=CARTESIAN_POINT('',(-1.47,0.42,-1.80023079474661E-16));
#15488=CARTESIAN_POINT('Origin',(0.,0.,0.));
#15489=CARTESIAN_POINT('',(-1.5,-0.39,-1.83697019872103E-16));
#15490=CARTESIAN_POINT('Origin',(0.,-0.39,0.));
#15491=CARTESIAN_POINT('',(-1.5,0.,-1.83697019872103E-16));
#15492=CARTESIAN_POINT('Origin',(0.,-0.42,0.));
#15493=CARTESIAN_POINT('',(-1.44,-0.45,-1.76349139077219E-16));
#15494=CARTESIAN_POINT('Origin',(0.,-0.45,0.));
#15495=CARTESIAN_POINT('',(-1.47,-0.42,-1.80023079474661E-16));
#15496=CARTESIAN_POINT('Origin',(1.023815,-0.45,0.));
#15497=CARTESIAN_POINT('Origin',(0.,0.,0.));
#15498=CARTESIAN_POINT('',(-1.023815,0.,-1.25381176266905E-16));
#15499=CARTESIAN_POINT('',(0.,0.,0.));
#15500=CARTESIAN_POINT('Origin',(1.,0.,0.));
#15501=CARTESIAN_POINT('',(1.,-1.78583896120461E-33,0.23815));
#15502=CARTESIAN_POINT('',(1.,-1.78583896120461E-33,-0.23815));
#15503=CARTESIAN_POINT('Origin',(1.,0.,0.));
#15504=CARTESIAN_POINT('Origin',(0.707106781186548,0.,-0.707106781186547));
#15505=CARTESIAN_POINT('',(0.875504261126124,-1.78583896120461E-33,-0.538709301246971));
#15506=CARTESIAN_POINT('',(0.538709301246971,-1.78583896120461E-33,-0.875504261126124));
#15507=CARTESIAN_POINT('Origin',(0.707106781186548,0.,-0.707106781186547));
#15508=CARTESIAN_POINT('Origin',(6.12323399573677E-17,0.,-1.));
#15509=CARTESIAN_POINT('',(0.23815,-1.78583896120461E-33,-1.));
#15510=CARTESIAN_POINT('',(-0.23815,-1.78583896120461E-33,-1.));
#15511=CARTESIAN_POINT('Origin',(6.12323399573677E-17,0.,-1.));
#15512=CARTESIAN_POINT('Origin',(-0.707106781186547,0.,-0.707106781186548));
#15513=CARTESIAN_POINT('',(-0.538709301246971,-1.78583896120461E-33,-0.875504261126124));
#15514=CARTESIAN_POINT('',(-0.875504261126124,-1.78583896120461E-33,-0.538709301246971));
#15515=CARTESIAN_POINT('Origin',(-0.707106781186547,0.,-0.707106781186548));
#15516=CARTESIAN_POINT('Origin',(-1.,0.,-1.22464679914735E-16));
#15517=CARTESIAN_POINT('',(-1.,-1.78583896120461E-33,-0.23815));
#15518=CARTESIAN_POINT('',(-1.,-1.78583896120461E-33,0.23815));
#15519=CARTESIAN_POINT('Origin',(-1.,0.,-1.22464679914735E-16));
#15520=CARTESIAN_POINT('Origin',(-0.707106781186548,0.,0.707106781186547));
#15521=CARTESIAN_POINT('',(-0.875504261126124,-7.94881478324376E-33,0.538709301246971));
#15522=CARTESIAN_POINT('',(-0.538709301246971,4.37713686083455E-33,0.875504261126124));
#15523=CARTESIAN_POINT('Origin',(-0.707106781186548,0.,0.707106781186547));
#15524=CARTESIAN_POINT('Origin',(-1.83697019872103E-16,0.,1.));
#15525=CARTESIAN_POINT('',(-0.23815,-1.78583896120461E-33,1.));
#15526=CARTESIAN_POINT('',(0.23815,-1.78583896120461E-33,1.));
#15527=CARTESIAN_POINT('Origin',(-1.83697019872103E-16,0.,1.));
#15528=CARTESIAN_POINT('Origin',(0.707106781186547,0.,0.707106781186548));
#15529=CARTESIAN_POINT('',(0.538709301246971,-4.86732687222419E-33,0.875504261126124));
#15530=CARTESIAN_POINT('',(0.875504261126124,1.29564894981497E-33,0.538709301246971));
#15531=CARTESIAN_POINT('Origin',(0.707106781186547,0.,0.707106781186548));
#15532=CARTESIAN_POINT('',(0.,0.,0.));
#15533=CARTESIAN_POINT('Origin',(0.707106781186547,0.,0.707106781186548));
#15534=CARTESIAN_POINT('',(0.504455939115715,-0.04763,0.841298510752802));
#15535=CARTESIAN_POINT('',(0.841298510752802,-0.04763,0.504455939115715));
#15536=CARTESIAN_POINT('Ctrl Pts',(0.504455939115715,-0.04763,0.841298510752802));
#15537=CARTESIAN_POINT('Ctrl Pts',(0.508899795931835,-0.0740444353928835,
0.838633903678357));
#15538=CARTESIAN_POINT('Ctrl Pts',(0.517157748491652,-0.0999305678883309,
0.833661031856294));
#15539=CARTESIAN_POINT('Ctrl Pts',(0.537715343527944,-0.142345102874864,
0.820511285096538));
#15540=CARTESIAN_POINT('Ctrl Pts',(0.548874290046456,-0.159766064500479,
0.813159949759));
#15541=CARTESIAN_POINT('Ctrl Pts',(0.573915184558107,-0.190326085855194,
0.795684265985089));
#15542=CARTESIAN_POINT('Ctrl Pts',(0.587792702767295,-0.203463743702801,
0.78555112003688));
#15543=CARTESIAN_POINT('Ctrl Pts',(0.615966552324775,-0.224161999508995,
0.763642258217233));
#15544=CARTESIAN_POINT('Ctrl Pts',(0.631684198665438,-0.232861760990032,
0.750785745543687));
#15545=CARTESIAN_POINT('Ctrl Pts',(0.663382628119203,-0.244251601209411,
0.722929908501543));
#15546=CARTESIAN_POINT('Ctrl Pts',(0.679352081686668,-0.246942143572133,
0.707917883896095));
#15547=CARTESIAN_POINT('Ctrl Pts',(0.707917883896095,-0.246942143572133,
0.679352081686668));
#15548=CARTESIAN_POINT('Ctrl Pts',(0.722929908501543,-0.244251601209411,
0.663382628119203));
#15549=CARTESIAN_POINT('Ctrl Pts',(0.750785745543687,-0.232861760990032,
0.631684198665439));
#15550=CARTESIAN_POINT('Ctrl Pts',(0.763642258217232,-0.224161999508995,
0.615966552324775));
#15551=CARTESIAN_POINT('Ctrl Pts',(0.78555112003688,-0.203463743702801,
0.587792702767295));
#15552=CARTESIAN_POINT('Ctrl Pts',(0.795684265985088,-0.190326085855194,
0.573915184558108));
#15553=CARTESIAN_POINT('Ctrl Pts',(0.813159949759,-0.15976606450048,0.548874290046456));
#15554=CARTESIAN_POINT('Ctrl Pts',(0.820511285096538,-0.142345102874864,
0.537715343527944));
#15555=CARTESIAN_POINT('Ctrl Pts',(0.833661031856294,-0.099930567888331,
0.517157748491653));
#15556=CARTESIAN_POINT('Ctrl Pts',(0.838633903678357,-0.0740444353928835,
0.508899795931835));
#15557=CARTESIAN_POINT('Ctrl Pts',(0.841298510752801,-0.0476299999999999,
0.504455939115715));
#15558=CARTESIAN_POINT('',(0.528110872004958,-0.04763,0.871530771444223));
#15559=CARTESIAN_POINT('Origin',(0.707106781186547,-0.04763,0.707106781186548));
#15560=CARTESIAN_POINT('',(0.871530771444223,-0.04763,0.528110872004959));
#15561=CARTESIAN_POINT('Ctrl Pts',(0.871530771444223,-0.0476300000000001,
0.528110872004958));
#15562=CARTESIAN_POINT('Ctrl Pts',(0.87014664509073,-0.0609922781173483,
0.530395067942936));
#15563=CARTESIAN_POINT('Ctrl Pts',(0.868149331745851,-0.0742967091364493,
0.533674141594226));
#15564=CARTESIAN_POINT('Ctrl Pts',(0.85981294420286,-0.115492077056649,
0.54708917182331));
#15565=CARTESIAN_POINT('Ctrl Pts',(0.850993704737257,-0.141695629206859,
0.560922177770136));
#15566=CARTESIAN_POINT('Ctrl Pts',(0.830754510485543,-0.181890537957859,
0.590422647829571));
#15567=CARTESIAN_POINT('Ctrl Pts',(0.816896541396381,-0.201072148666545,
0.609616703125488));
#15568=CARTESIAN_POINT('Ctrl Pts',(0.792310597819928,-0.223955109275652,
0.641117951819998));
#15569=CARTESIAN_POINT('Ctrl Pts',(0.779109323683612,-0.232742381310829,
0.657208095763053));
#15570=CARTESIAN_POINT('Ctrl Pts',(0.750552691816206,-0.244234834628584,
0.68964083160521));
#15571=CARTESIAN_POINT('Ctrl Pts',(0.735185187071673,-0.246942143572133,
0.705971972091755));
#15572=CARTESIAN_POINT('Ctrl Pts',(0.705971972091754,-0.246942143572133,
0.735185187071673));
#15573=CARTESIAN_POINT('Ctrl Pts',(0.689640831605209,-0.244234834628584,
0.750552691816206));
#15574=CARTESIAN_POINT('Ctrl Pts',(0.657208095763052,-0.232742381310829,
0.779109323683612));
#15575=CARTESIAN_POINT('Ctrl Pts',(0.641117951819998,-0.223955109275652,
0.792310597819928));
#15576=CARTESIAN_POINT('Ctrl Pts',(0.609616703125487,-0.201072148666545,
0.816896541396382));
#15577=CARTESIAN_POINT('Ctrl Pts',(0.590422647829571,-0.181890537957858,
0.830754510485544));
#15578=CARTESIAN_POINT('Ctrl Pts',(0.560922177770135,-0.141695629206858,
0.850993704737257));
#15579=CARTESIAN_POINT('Ctrl Pts',(0.547089171823309,-0.115492077056649,
0.859812944202861));
#15580=CARTESIAN_POINT('Ctrl Pts',(0.533674141594226,-0.0742967091364491,
0.868149331745852));
#15581=CARTESIAN_POINT('Ctrl Pts',(0.530395067942936,-0.0609922781173483,
0.870146645090731));
#15582=CARTESIAN_POINT('Ctrl Pts',(0.528110872004958,-0.0476300000000001,
0.871530771444223));
#15583=CARTESIAN_POINT('Origin',(0.707106781186547,-0.04763,0.707106781186548));
#15584=CARTESIAN_POINT('Origin',(0.,-0.166705,0.));
#15585=CARTESIAN_POINT('',(0.242834539687906,-0.04763,0.989696097314));
#15586=CARTESIAN_POINT('Origin',(0.,-0.04763,0.));
#15587=CARTESIAN_POINT('',(-0.242834539687907,-0.04763,0.989696097314));
#15588=CARTESIAN_POINT('Ctrl Pts',(0.242834539687906,-0.04763,0.989696097314));
#15589=CARTESIAN_POINT('Ctrl Pts',(0.24024064412003,-0.0609922781173483,
0.990332542620729));
#15590=CARTESIAN_POINT('Ctrl Pts',(0.236509675094874,-0.0742967091364492,
0.991238884025248));
#15591=CARTESIAN_POINT('Ctrl Pts',(0.221129100087819,-0.115492077056649,
0.994830026707808));
#15592=CARTESIAN_POINT('Ctrl Pts',(0.205111543747588,-0.141695629206859,
0.998375294985966));
#15593=CARTESIAN_POINT('Ctrl Pts',(0.169940289819232,-0.181890537957859,
1.00492400591205));
#15594=CARTESIAN_POINT('Ctrl Pts',(0.1465689792446,-0.201072148666545,1.00869718865384));
#15595=CARTESIAN_POINT('Ctrl Pts',(0.106909345252087,-0.223955109275652,
1.01358704779679));
#15596=CARTESIAN_POINT('Ctrl Pts',(0.0861971848975941,-0.232742381310829,
1.0156297872271));
#15597=CARTESIAN_POINT('Ctrl Pts',(0.0430711894098822,-0.244234834628584,
1.01837060663223));
#15598=CARTESIAN_POINT('Ctrl Pts',(0.0206568624125605,-0.246942143572133,
1.019052));
#15599=CARTESIAN_POINT('Ctrl Pts',(-0.0206568624125608,-0.246942143572133,
1.019052));
#15600=CARTESIAN_POINT('Ctrl Pts',(-0.0430711894098825,-0.244234834628584,
1.01837060663223));
#15601=CARTESIAN_POINT('Ctrl Pts',(-0.0861971848975943,-0.232742381310829,
1.0156297872271));
#15602=CARTESIAN_POINT('Ctrl Pts',(-0.106909345252088,-0.223955109275652,
1.01358704779679));
#15603=CARTESIAN_POINT('Ctrl Pts',(-0.1465689792446,-0.201072148666545,
1.00869718865384));
#15604=CARTESIAN_POINT('Ctrl Pts',(-0.169940289819232,-0.181890537957859,
1.00492400591205));
#15605=CARTESIAN_POINT('Ctrl Pts',(-0.205111543747588,-0.141695629206859,
0.998375294985966));
#15606=CARTESIAN_POINT('Ctrl Pts',(-0.221129100087819,-0.115492077056649,
0.994830026707808));
#15607=CARTESIAN_POINT('Ctrl Pts',(-0.236509675094875,-0.0742967091364493,
0.991238884025248));
#15608=CARTESIAN_POINT('Ctrl Pts',(-0.24024064412003,-0.0609922781173483,
0.990332542620729));
#15609=CARTESIAN_POINT('Ctrl Pts',(-0.242834539687907,-0.04763,0.989696097314));
#15610=CARTESIAN_POINT('',(-0.528110872004959,-0.04763,0.871530771444223));
#15611=CARTESIAN_POINT('Origin',(0.,-0.04763,0.));
#15612=CARTESIAN_POINT('',(-0.871530771444223,-0.04763,0.528110872004958));
#15613=CARTESIAN_POINT('Ctrl Pts',(-0.528110872004958,-0.0476300000000001,
0.871530771444223));
#15614=CARTESIAN_POINT('Ctrl Pts',(-0.530395067942936,-0.0609922781173484,
0.87014664509073));
#15615=CARTESIAN_POINT('Ctrl Pts',(-0.533674141594226,-0.0742967091364493,
0.868149331745851));
#15616=CARTESIAN_POINT('Ctrl Pts',(-0.54708917182331,-0.115492077056649,
0.85981294420286));
#15617=CARTESIAN_POINT('Ctrl Pts',(-0.560922177770136,-0.141695629206859,
0.850993704737257));
#15618=CARTESIAN_POINT('Ctrl Pts',(-0.590422647829571,-0.181890537957859,
0.830754510485543));
#15619=CARTESIAN_POINT('Ctrl Pts',(-0.609616703125488,-0.201072148666545,
0.816896541396381));
#15620=CARTESIAN_POINT('Ctrl Pts',(-0.641117951819998,-0.223955109275652,
0.792310597819928));
#15621=CARTESIAN_POINT('Ctrl Pts',(-0.657208095763053,-0.232742381310829,
0.779109323683611));
#15622=CARTESIAN_POINT('Ctrl Pts',(-0.68964083160521,-0.244234834628584,
0.750552691816205));
#15623=CARTESIAN_POINT('Ctrl Pts',(-0.705971972091755,-0.246942143572133,
0.735185187071673));
#15624=CARTESIAN_POINT('Ctrl Pts',(-0.735185187071673,-0.246942143572133,
0.705971972091754));
#15625=CARTESIAN_POINT('Ctrl Pts',(-0.750552691816206,-0.244234834628584,
0.689640831605209));
#15626=CARTESIAN_POINT('Ctrl Pts',(-0.779109323683612,-0.232742381310829,
0.657208095763052));
#15627=CARTESIAN_POINT('Ctrl Pts',(-0.792310597819928,-0.223955109275652,
0.641117951819998));
#15628=CARTESIAN_POINT('Ctrl Pts',(-0.816896541396382,-0.201072148666545,
0.609616703125487));
#15629=CARTESIAN_POINT('Ctrl Pts',(-0.830754510485544,-0.181890537957858,
0.590422647829571));
#15630=CARTESIAN_POINT('Ctrl Pts',(-0.850993704737257,-0.141695629206858,
0.560922177770135));
#15631=CARTESIAN_POINT('Ctrl Pts',(-0.859812944202861,-0.115492077056649,
0.547089171823309));
#15632=CARTESIAN_POINT('Ctrl Pts',(-0.868149331745852,-0.0742967091364491,
0.533674141594226));
#15633=CARTESIAN_POINT('Ctrl Pts',(-0.870146645090731,-0.0609922781173483,
0.530395067942936));
#15634=CARTESIAN_POINT('Ctrl Pts',(-0.871530771444223,-0.04763,0.528110872004958));
#15635=CARTESIAN_POINT('',(-0.989696097314,-0.04763,0.242834539687906));
#15636=CARTESIAN_POINT('Origin',(0.,-0.04763,0.));
#15637=CARTESIAN_POINT('',(-1.019052,-0.246942143572133,1.248489836334E-16));
#15638=CARTESIAN_POINT('Ctrl Pts',(-0.989696097314,-0.04763,0.242834539687906));
#15639=CARTESIAN_POINT('Ctrl Pts',(-0.990332542620729,-0.0609922781173483,
0.24024064412003));
#15640=CARTESIAN_POINT('Ctrl Pts',(-0.991238884025248,-0.0742967091364492,
0.236509675094874));
#15641=CARTESIAN_POINT('Ctrl Pts',(-0.994830026707808,-0.115492077056649,
0.221129100087819));
#15642=CARTESIAN_POINT('Ctrl Pts',(-0.998375294985966,-0.141695629206859,
0.205111543747588));
#15643=CARTESIAN_POINT('Ctrl Pts',(-1.00492400591205,-0.181890537957859,
0.169940289819232));
#15644=CARTESIAN_POINT('Ctrl Pts',(-1.00869718865384,-0.201072148666545,
0.1465689792446));
#15645=CARTESIAN_POINT('Ctrl Pts',(-1.01358704779679,-0.223955109275652,
0.106909345252088));
#15646=CARTESIAN_POINT('Ctrl Pts',(-1.0156297872271,-0.232742381310829,
0.0861971848975944));
#15647=CARTESIAN_POINT('Ctrl Pts',(-1.01837060663223,-0.244234834628584,
0.0430711894098825));
#15648=CARTESIAN_POINT('Ctrl Pts',(-1.019052,-0.246942143572133,0.0206568624125608));
#15649=CARTESIAN_POINT('Ctrl Pts',(-1.019052,-0.246942143572133,1.2490009027033E-16));
#15650=CARTESIAN_POINT('',(-1.019052,-0.28578,1.24797876996471E-16));
#15651=CARTESIAN_POINT('',(-1.019052,-0.166705,1.24797876996471E-16));
#15652=CARTESIAN_POINT('Origin',(0.,-0.28578,0.));
#15653=CARTESIAN_POINT('',(-0.989696097314,-0.04763,-0.242834539687906));
#15654=CARTESIAN_POINT('Ctrl Pts',(-1.019052,-0.246942143572133,1.2490009027033E-16));
#15655=CARTESIAN_POINT('Ctrl Pts',(-1.019052,-0.246942143572133,-0.0206568624125605));
#15656=CARTESIAN_POINT('Ctrl Pts',(-1.01837060663223,-0.244234834628584,
-0.0430711894098822));
#15657=CARTESIAN_POINT('Ctrl Pts',(-1.0156297872271,-0.232742381310829,
-0.0861971848975941));
#15658=CARTESIAN_POINT('Ctrl Pts',(-1.01358704779679,-0.223955109275652,
-0.106909345252087));
#15659=CARTESIAN_POINT('Ctrl Pts',(-1.00869718865384,-0.201072148666546,
-0.1465689792446));
#15660=CARTESIAN_POINT('Ctrl Pts',(-1.00492400591205,-0.181890537957859,
-0.169940289819232));
#15661=CARTESIAN_POINT('Ctrl Pts',(-0.998375294985966,-0.141695629206859,
-0.205111543747588));
#15662=CARTESIAN_POINT('Ctrl Pts',(-0.994830026707808,-0.11549207705665,
-0.221129100087819));
#15663=CARTESIAN_POINT('Ctrl Pts',(-0.991238884025248,-0.0742967091364495,
-0.236509675094874));
#15664=CARTESIAN_POINT('Ctrl Pts',(-0.990332542620729,-0.0609922781173484,
-0.24024064412003));
#15665=CARTESIAN_POINT('Ctrl Pts',(-0.989696097314,-0.0476300000000001,
-0.242834539687907));
#15666=CARTESIAN_POINT('',(-0.871530771444223,-0.04763,-0.528110872004958));
#15667=CARTESIAN_POINT('Origin',(0.,-0.04763,0.));
#15668=CARTESIAN_POINT('',(-0.528110872004958,-0.04763,-0.871530771444223));
#15669=CARTESIAN_POINT('Ctrl Pts',(-0.871530771444223,-0.0476300000000001,
-0.528110872004958));
#15670=CARTESIAN_POINT('Ctrl Pts',(-0.87014664509073,-0.0609922781173484,
-0.530395067942936));
#15671=CARTESIAN_POINT('Ctrl Pts',(-0.868149331745851,-0.0742967091364494,
-0.533674141594226));
#15672=CARTESIAN_POINT('Ctrl Pts',(-0.85981294420286,-0.115492077056649,
-0.54708917182331));
#15673=CARTESIAN_POINT('Ctrl Pts',(-0.850993704737257,-0.141695629206859,
-0.560922177770136));
#15674=CARTESIAN_POINT('Ctrl Pts',(-0.830754510485543,-0.181890537957859,
-0.590422647829571));
#15675=CARTESIAN_POINT('Ctrl Pts',(-0.816896541396381,-0.201072148666546,
-0.609616703125488));
#15676=CARTESIAN_POINT('Ctrl Pts',(-0.792310597819928,-0.223955109275652,
-0.641117951819999));
#15677=CARTESIAN_POINT('Ctrl Pts',(-0.779109323683611,-0.232742381310829,
-0.657208095763053));
#15678=CARTESIAN_POINT('Ctrl Pts',(-0.750552691816205,-0.244234834628584,
-0.68964083160521));
#15679=CARTESIAN_POINT('Ctrl Pts',(-0.735185187071673,-0.246942143572133,
-0.705971972091755));
#15680=CARTESIAN_POINT('Ctrl Pts',(-0.705971972091754,-0.246942143572133,
-0.735185187071673));
#15681=CARTESIAN_POINT('Ctrl Pts',(-0.68964083160521,-0.244234834628584,
-0.750552691816206));
#15682=CARTESIAN_POINT('Ctrl Pts',(-0.657208095763052,-0.232742381310829,
-0.779109323683612));
#15683=CARTESIAN_POINT('Ctrl Pts',(-0.641117951819998,-0.223955109275652,
-0.792310597819928));
#15684=CARTESIAN_POINT('Ctrl Pts',(-0.609616703125488,-0.201072148666545,
-0.816896541396381));
#15685=CARTESIAN_POINT('Ctrl Pts',(-0.590422647829571,-0.181890537957859,
-0.830754510485543));
#15686=CARTESIAN_POINT('Ctrl Pts',(-0.560922177770136,-0.141695629206859,
-0.850993704737257));
#15687=CARTESIAN_POINT('Ctrl Pts',(-0.54708917182331,-0.115492077056649,
-0.85981294420286));
#15688=CARTESIAN_POINT('Ctrl Pts',(-0.533674141594226,-0.0742967091364494,
-0.868149331745852));
#15689=CARTESIAN_POINT('Ctrl Pts',(-0.530395067942936,-0.0609922781173484,
-0.870146645090731));
#15690=CARTESIAN_POINT('Ctrl Pts',(-0.528110872004958,-0.0476300000000001,
-0.871530771444223));
#15691=CARTESIAN_POINT('',(-0.242834539687906,-0.04763,-0.989696097314));
#15692=CARTESIAN_POINT('Origin',(0.,-0.04763,0.));
#15693=CARTESIAN_POINT('',(0.242834539687906,-0.04763,-0.989696097314));
#15694=CARTESIAN_POINT('Ctrl Pts',(-0.242834539687907,-0.04763,-0.989696097314));
#15695=CARTESIAN_POINT('Ctrl Pts',(-0.24024064412003,-0.0609922781173483,
-0.990332542620729));
#15696=CARTESIAN_POINT('Ctrl Pts',(-0.236509675094874,-0.0742967091364493,
-0.991238884025248));
#15697=CARTESIAN_POINT('Ctrl Pts',(-0.221129100087819,-0.115492077056649,
-0.994830026707808));
#15698=CARTESIAN_POINT('Ctrl Pts',(-0.205111543747588,-0.141695629206859,
-0.998375294985966));
#15699=CARTESIAN_POINT('Ctrl Pts',(-0.169940289819232,-0.181890537957859,
-1.00492400591205));
#15700=CARTESIAN_POINT('Ctrl Pts',(-0.1465689792446,-0.201072148666545,
-1.00869718865384));
#15701=CARTESIAN_POINT('Ctrl Pts',(-0.106909345252087,-0.223955109275652,
-1.01358704779679));
#15702=CARTESIAN_POINT('Ctrl Pts',(-0.0861971848975942,-0.232742381310829,
-1.0156297872271));
#15703=CARTESIAN_POINT('Ctrl Pts',(-0.0430711894098823,-0.244234834628584,
-1.01837060663223));
#15704=CARTESIAN_POINT('Ctrl Pts',(-0.0206568624125606,-0.246942143572133,
-1.019052));
#15705=CARTESIAN_POINT('Ctrl Pts',(0.0206568624125607,-0.246942143572133,
-1.019052));
#15706=CARTESIAN_POINT('Ctrl Pts',(0.0430711894098824,-0.244234834628584,
-1.01837060663223));
#15707=CARTESIAN_POINT('Ctrl Pts',(0.0861971848975943,-0.232742381310829,
-1.0156297872271));
#15708=CARTESIAN_POINT('Ctrl Pts',(0.106909345252088,-0.223955109275652,
-1.01358704779679));
#15709=CARTESIAN_POINT('Ctrl Pts',(0.1465689792446,-0.201072148666545,-1.00869718865384));
#15710=CARTESIAN_POINT('Ctrl Pts',(0.169940289819232,-0.181890537957859,
-1.00492400591205));
#15711=CARTESIAN_POINT('Ctrl Pts',(0.205111543747588,-0.141695629206859,
-0.998375294985966));
#15712=CARTESIAN_POINT('Ctrl Pts',(0.221129100087819,-0.115492077056649,
-0.994830026707808));
#15713=CARTESIAN_POINT('Ctrl Pts',(0.236509675094874,-0.0742967091364493,
-0.991238884025248));
#15714=CARTESIAN_POINT('Ctrl Pts',(0.24024064412003,-0.0609922781173484,
-0.990332542620729));
#15715=CARTESIAN_POINT('Ctrl Pts',(0.242834539687907,-0.04763,-0.989696097314));
#15716=CARTESIAN_POINT('',(0.528110872004958,-0.04763,-0.871530771444223));
#15717=CARTESIAN_POINT('Origin',(0.,-0.04763,0.));
#15718=CARTESIAN_POINT('',(0.871530771444223,-0.04763,-0.528110872004958));
#15719=CARTESIAN_POINT('Ctrl Pts',(0.528110872004958,-0.0476300000000001,
-0.871530771444223));
#15720=CARTESIAN_POINT('Ctrl Pts',(0.530395067942936,-0.0609922781173484,
-0.870146645090731));
#15721=CARTESIAN_POINT('Ctrl Pts',(0.533674141594226,-0.0742967091364493,
-0.868149331745851));
#15722=CARTESIAN_POINT('Ctrl Pts',(0.54708917182331,-0.115492077056649,
-0.85981294420286));
#15723=CARTESIAN_POINT('Ctrl Pts',(0.560922177770136,-0.141695629206859,
-0.850993704737257));
#15724=CARTESIAN_POINT('Ctrl Pts',(0.590422647829571,-0.181890537957859,
-0.830754510485543));
#15725=CARTESIAN_POINT('Ctrl Pts',(0.609616703125488,-0.201072148666545,
-0.816896541396381));
#15726=CARTESIAN_POINT('Ctrl Pts',(0.641117951819998,-0.223955109275652,
-0.792310597819928));
#15727=CARTESIAN_POINT('Ctrl Pts',(0.657208095763053,-0.232742381310829,
-0.779109323683612));
#15728=CARTESIAN_POINT('Ctrl Pts',(0.68964083160521,-0.244234834628584,
-0.750552691816206));
#15729=CARTESIAN_POINT('Ctrl Pts',(0.705971972091755,-0.246942143572133,
-0.735185187071673));
#15730=CARTESIAN_POINT('Ctrl Pts',(0.735185187071673,-0.246942143572133,
-0.705971972091754));
#15731=CARTESIAN_POINT('Ctrl Pts',(0.750552691816206,-0.244234834628584,
-0.68964083160521));
#15732=CARTESIAN_POINT('Ctrl Pts',(0.779109323683612,-0.232742381310829,
-0.657208095763053));
#15733=CARTESIAN_POINT('Ctrl Pts',(0.792310597819928,-0.223955109275652,
-0.641117951819998));
#15734=CARTESIAN_POINT('Ctrl Pts',(0.816896541396381,-0.201072148666545,
-0.609616703125488));
#15735=CARTESIAN_POINT('Ctrl Pts',(0.830754510485543,-0.181890537957859,
-0.590422647829571));
#15736=CARTESIAN_POINT('Ctrl Pts',(0.850993704737257,-0.141695629206859,
-0.560922177770136));
#15737=CARTESIAN_POINT('Ctrl Pts',(0.85981294420286,-0.115492077056649,
-0.54708917182331));
#15738=CARTESIAN_POINT('Ctrl Pts',(0.868149331745851,-0.0742967091364493,
-0.533674141594226));
#15739=CARTESIAN_POINT('Ctrl Pts',(0.870146645090731,-0.0609922781173484,
-0.530395067942936));
#15740=CARTESIAN_POINT('Ctrl Pts',(0.871530771444223,-0.0476300000000001,
-0.528110872004958));
#15741=CARTESIAN_POINT('',(0.989696097314,-0.04763,-0.242834539687906));
#15742=CARTESIAN_POINT('Origin',(0.,-0.04763,0.));
#15743=CARTESIAN_POINT('',(0.989696097314,-0.04763,0.242834539687906));
#15744=CARTESIAN_POINT('Ctrl Pts',(0.989696097314,-0.04763,-0.242834539687907));
#15745=CARTESIAN_POINT('Ctrl Pts',(0.990332542620729,-0.0609922781173483,
-0.24024064412003));
#15746=CARTESIAN_POINT('Ctrl Pts',(0.991238884025248,-0.0742967091364493,
-0.236509675094874));
#15747=CARTESIAN_POINT('Ctrl Pts',(0.994830026707808,-0.115492077056649,
-0.221129100087819));
#15748=CARTESIAN_POINT('Ctrl Pts',(0.998375294985966,-0.141695629206859,
-0.205111543747588));
#15749=CARTESIAN_POINT('Ctrl Pts',(1.00492400591205,-0.181890537957859,
-0.169940289819232));
#15750=CARTESIAN_POINT('Ctrl Pts',(1.00869718865384,-0.201072148666545,
-0.1465689792446));
#15751=CARTESIAN_POINT('Ctrl Pts',(1.01358704779679,-0.223955109275652,
-0.106909345252087));
#15752=CARTESIAN_POINT('Ctrl Pts',(1.0156297872271,-0.232742381310829,-0.0861971848975942));
#15753=CARTESIAN_POINT('Ctrl Pts',(1.01837060663223,-0.244234834628584,
-0.0430711894098823));
#15754=CARTESIAN_POINT('Ctrl Pts',(1.019052,-0.246942143572133,-0.0206568624125607));
#15755=CARTESIAN_POINT('Ctrl Pts',(1.019052,-0.246942143572133,0.0206568624125607));
#15756=CARTESIAN_POINT('Ctrl Pts',(1.01837060663223,-0.244234834628584,
0.0430711894098823));
#15757=CARTESIAN_POINT('Ctrl Pts',(1.0156297872271,-0.232742381310829,0.0861971848975942));
#15758=CARTESIAN_POINT('Ctrl Pts',(1.01358704779679,-0.223955109275652,
0.106909345252087));
#15759=CARTESIAN_POINT('Ctrl Pts',(1.00869718865384,-0.201072148666545,
0.1465689792446));
#15760=CARTESIAN_POINT('Ctrl Pts',(1.00492400591205,-0.181890537957859,
0.169940289819232));
#15761=CARTESIAN_POINT('Ctrl Pts',(0.998375294985966,-0.141695629206859,
0.205111543747588));
#15762=CARTESIAN_POINT('Ctrl Pts',(0.994830026707808,-0.115492077056649,
0.221129100087819));
#15763=CARTESIAN_POINT('Ctrl Pts',(0.991238884025248,-0.0742967091364492,
0.236509675094874));
#15764=CARTESIAN_POINT('Ctrl Pts',(0.990332542620729,-0.0609922781173483,
0.24024064412003));
#15765=CARTESIAN_POINT('Ctrl Pts',(0.989696097314,-0.04763,0.242834539687907));
#15766=CARTESIAN_POINT('Origin',(0.,-0.04763,0.));
#15767=CARTESIAN_POINT('Origin',(0.,-0.04763,0.));
#15768=CARTESIAN_POINT('',(0.238183666596899,-0.04763,0.951592097314));
#15769=CARTESIAN_POINT('Origin',(0.,-0.04763,0.));
#15770=CARTESIAN_POINT('Origin',(-1.94289029309402E-16,-0.04763,1.));
#15771=CARTESIAN_POINT('Origin',(-1.94289029309402E-16,0.,1.));
#15772=CARTESIAN_POINT('',(-0.2381836665969,-0.04763,0.951592097314));
#15773=CARTESIAN_POINT('Ctrl Pts',(-0.238183666596899,-0.0476299999999999,
0.951592097314));
#15774=CARTESIAN_POINT('Ctrl Pts',(-0.233157223576062,-0.0740444353928835,
0.952850216871763));
#15775=CARTESIAN_POINT('Ctrl Pts',(-0.223801617934946,-0.0999305678883309,
0.955173119738174));
#15776=CARTESIAN_POINT('Ctrl Pts',(-0.199966927975188,-0.142345102874864,
0.960411259488514));
#15777=CARTESIAN_POINT('Ctrl Pts',(-0.1868781821531,-0.159766064500479,
0.963103647174702));
#15778=CARTESIAN_POINT('Ctrl Pts',(-0.15681442133453,-0.190326085855194,
0.968453058988463));
#15779=CARTESIAN_POINT('Ctrl Pts',(-0.139836317888043,-0.203463743702801,
0.971100730005489));
#15780=CARTESIAN_POINT('Ctrl Pts',(-0.104422493053067,-0.224161999508995,
0.975530745318961));
#15781=CARTESIAN_POINT('Ctrl Pts',(-0.0842175114474176,-0.232861760990032,
0.977553872336861));
#15782=CARTESIAN_POINT('Ctrl Pts',(-0.0421062857595701,-0.244251601209411,
0.980270995488453));
#15783=CARTESIAN_POINT('Ctrl Pts',(-0.0201990724523197,-0.246942143572133,
0.980948));
#15784=CARTESIAN_POINT('Ctrl Pts',(0.020199072452319,-0.246942143572133,
0.980948));
#15785=CARTESIAN_POINT('Ctrl Pts',(0.0421062857595694,-0.244251601209411,
0.980270995488454));
#15786=CARTESIAN_POINT('Ctrl Pts',(0.0842175114474169,-0.232861760990032,
0.977553872336861));
#15787=CARTESIAN_POINT('Ctrl Pts',(0.104422493053067,-0.224161999508995,
0.975530745318961));
#15788=CARTESIAN_POINT('Ctrl Pts',(0.139836317888042,-0.203463743702801,
0.971100730005489));
#15789=CARTESIAN_POINT('Ctrl Pts',(0.15681442133453,-0.190326085855194,
0.968453058988463));
#15790=CARTESIAN_POINT('Ctrl Pts',(0.1868781821531,-0.15976606450048,0.963103647174702));
#15791=CARTESIAN_POINT('Ctrl Pts',(0.199966927975188,-0.142345102874864,
0.960411259488514));
#15792=CARTESIAN_POINT('Ctrl Pts',(0.223801617934945,-0.0999305678883309,
0.955173119738174));
#15793=CARTESIAN_POINT('Ctrl Pts',(0.233157223576061,-0.0740444353928835,
0.952850216871763));
#15794=CARTESIAN_POINT('Ctrl Pts',(0.238183666596899,-0.0476299999999999,
0.951592097314));
#15795=CARTESIAN_POINT('Origin',(-1.94289029309402E-16,-0.04763,1.));
#15796=CARTESIAN_POINT('Origin',(0.,-0.04763,0.));
#15797=CARTESIAN_POINT('',(-0.504455939115715,-0.04763,0.841298510752802));
#15798=CARTESIAN_POINT('Origin',(0.,-0.04763,0.));
#15799=CARTESIAN_POINT('Origin',(-0.707106781186548,-0.04763,0.707106781186547));
#15800=CARTESIAN_POINT('Origin',(-0.707106781186548,0.,0.707106781186547));
#15801=CARTESIAN_POINT('',(-0.841298510752802,-0.04763,0.504455939115715));
#15802=CARTESIAN_POINT('Ctrl Pts',(-0.841298510752802,-0.04763,0.504455939115715));
#15803=CARTESIAN_POINT('Ctrl Pts',(-0.838633903678357,-0.0740444353928835,
0.508899795931835));
#15804=CARTESIAN_POINT('Ctrl Pts',(-0.833661031856294,-0.0999305678883309,
0.517157748491652));
#15805=CARTESIAN_POINT('Ctrl Pts',(-0.820511285096538,-0.142345102874864,
0.537715343527944));
#15806=CARTESIAN_POINT('Ctrl Pts',(-0.813159949759,-0.159766064500479,0.548874290046456));
#15807=CARTESIAN_POINT('Ctrl Pts',(-0.795684265985089,-0.190326085855194,
0.573915184558107));
#15808=CARTESIAN_POINT('Ctrl Pts',(-0.78555112003688,-0.203463743702801,
0.587792702767295));
#15809=CARTESIAN_POINT('Ctrl Pts',(-0.763642258217233,-0.224161999508995,
0.615966552324775));
#15810=CARTESIAN_POINT('Ctrl Pts',(-0.750785745543687,-0.232861760990032,
0.631684198665438));
#15811=CARTESIAN_POINT('Ctrl Pts',(-0.722929908501543,-0.244251601209411,
0.663382628119203));
#15812=CARTESIAN_POINT('Ctrl Pts',(-0.707917883896095,-0.246942143572133,
0.679352081686668));
#15813=CARTESIAN_POINT('Ctrl Pts',(-0.679352081686668,-0.246942143572133,
0.707917883896095));
#15814=CARTESIAN_POINT('Ctrl Pts',(-0.663382628119203,-0.244251601209411,
0.722929908501544));
#15815=CARTESIAN_POINT('Ctrl Pts',(-0.631684198665438,-0.232861760990031,
0.750785745543687));
#15816=CARTESIAN_POINT('Ctrl Pts',(-0.615966552324775,-0.224161999508995,
0.763642258217233));
#15817=CARTESIAN_POINT('Ctrl Pts',(-0.587792702767295,-0.203463743702801,
0.78555112003688));
#15818=CARTESIAN_POINT('Ctrl Pts',(-0.573915184558107,-0.190326085855194,
0.795684265985088));
#15819=CARTESIAN_POINT('Ctrl Pts',(-0.548874290046456,-0.159766064500479,
0.813159949759));
#15820=CARTESIAN_POINT('Ctrl Pts',(-0.537715343527944,-0.142345102874864,
0.820511285096538));
#15821=CARTESIAN_POINT('Ctrl Pts',(-0.517157748491652,-0.0999305678883309,
0.833661031856294));
#15822=CARTESIAN_POINT('Ctrl Pts',(-0.508899795931835,-0.0740444353928835,
0.838633903678357));
#15823=CARTESIAN_POINT('Ctrl Pts',(-0.504455939115716,-0.04763,0.841298510752801));
#15824=CARTESIAN_POINT('Origin',(-0.707106781186548,-0.04763,0.707106781186547));
#15825=CARTESIAN_POINT('Origin',(0.,-0.04763,0.));
#15826=CARTESIAN_POINT('',(-0.951592097314,-0.04763,0.238183666596899));
#15827=CARTESIAN_POINT('Origin',(0.,-0.04763,0.));
#15828=CARTESIAN_POINT('Origin',(-1.,-0.04763,-1.11022302462516E-16));
#15829=CARTESIAN_POINT('Origin',(-1.,0.,-1.11022302462516E-16));
#15830=CARTESIAN_POINT('',(-0.951592097314,-0.04763,-0.2381836665969));
#15831=CARTESIAN_POINT('',(-0.980948,-0.246942143572133,1.08514323328844E-18));
#15832=CARTESIAN_POINT('Ctrl Pts',(-0.951592097314,-0.04763,-0.238183666596899));
#15833=CARTESIAN_POINT('Ctrl Pts',(-0.952850216871763,-0.0740444353928835,
-0.233157223576062));
#15834=CARTESIAN_POINT('Ctrl Pts',(-0.955173119738174,-0.0999305678883309,
-0.223801617934946));
#15835=CARTESIAN_POINT('Ctrl Pts',(-0.960411259488514,-0.142345102874864,
-0.199966927975188));
#15836=CARTESIAN_POINT('Ctrl Pts',(-0.963103647174702,-0.159766064500479,
-0.1868781821531));
#15837=CARTESIAN_POINT('Ctrl Pts',(-0.968453058988463,-0.190326085855194,
-0.15681442133453));
#15838=CARTESIAN_POINT('Ctrl Pts',(-0.971100730005489,-0.203463743702801,
-0.139836317888043));
#15839=CARTESIAN_POINT('Ctrl Pts',(-0.975530745318961,-0.224161999508995,
-0.104422493053067));
#15840=CARTESIAN_POINT('Ctrl Pts',(-0.977553872336861,-0.232861760990032,
-0.0842175114474175));
#15841=CARTESIAN_POINT('Ctrl Pts',(-0.980270995488453,-0.244251601209411,
-0.0421062857595699));
#15842=CARTESIAN_POINT('Ctrl Pts',(-0.980948,-0.246942143572133,-0.0201990724523195));
#15843=CARTESIAN_POINT('Ctrl Pts',(-0.980948,-0.246942143572133,-1.17961196366423E-16));
#15844=CARTESIAN_POINT('Origin',(-1.,-0.04763,-1.11022302462516E-16));
#15845=CARTESIAN_POINT('Ctrl Pts',(-0.980948,-0.246942143572133,-1.17961196366423E-16));
#15846=CARTESIAN_POINT('Ctrl Pts',(-0.980948,-0.246942143572133,0.0201990724523192));
#15847=CARTESIAN_POINT('Ctrl Pts',(-0.980270995488453,-0.244251601209411,
0.0421062857595695));
#15848=CARTESIAN_POINT('Ctrl Pts',(-0.977553872336861,-0.232861760990032,
0.0842175114474169));
#15849=CARTESIAN_POINT('Ctrl Pts',(-0.975530745318961,-0.224161999508995,
0.104422493053066));
#15850=CARTESIAN_POINT('Ctrl Pts',(-0.971100730005489,-0.203463743702801,
0.139836317888042));
#15851=CARTESIAN_POINT('Ctrl Pts',(-0.968453058988463,-0.190326085855194,
0.15681442133453));
#15852=CARTESIAN_POINT('Ctrl Pts',(-0.963103647174702,-0.15976606450048,
0.1868781821531));
#15853=CARTESIAN_POINT('Ctrl Pts',(-0.960411259488514,-0.142345102874864,
0.199966927975188));
#15854=CARTESIAN_POINT('Ctrl Pts',(-0.955173119738174,-0.099930567888331,
0.223801617934945));
#15855=CARTESIAN_POINT('Ctrl Pts',(-0.952850216871763,-0.0740444353928835,
0.233157223576061));
#15856=CARTESIAN_POINT('Ctrl Pts',(-0.951592097314,-0.04763,0.238183666596899));
#15857=CARTESIAN_POINT('Origin',(0.,-0.04763,0.));
#15858=CARTESIAN_POINT('',(-0.841298510752802,-0.04763,-0.504455939115715));
#15859=CARTESIAN_POINT('Origin',(0.,-0.04763,0.));
#15860=CARTESIAN_POINT('Origin',(-0.707106781186547,-0.04763,-0.707106781186548));
#15861=CARTESIAN_POINT('Origin',(-0.707106781186547,0.,-0.707106781186548));
#15862=CARTESIAN_POINT('',(-0.504455939115715,-0.04763,-0.841298510752802));
#15863=CARTESIAN_POINT('Ctrl Pts',(-0.504455939115715,-0.04763,-0.841298510752802));
#15864=CARTESIAN_POINT('Ctrl Pts',(-0.508899795931835,-0.0740444353928835,
-0.838633903678357));
#15865=CARTESIAN_POINT('Ctrl Pts',(-0.517157748491652,-0.0999305678883309,
-0.833661031856294));
#15866=CARTESIAN_POINT('Ctrl Pts',(-0.537715343527944,-0.142345102874864,
-0.820511285096538));
#15867=CARTESIAN_POINT('Ctrl Pts',(-0.548874290046456,-0.159766064500479,
-0.813159949759));
#15868=CARTESIAN_POINT('Ctrl Pts',(-0.573915184558107,-0.190326085855194,
-0.795684265985089));
#15869=CARTESIAN_POINT('Ctrl Pts',(-0.587792702767295,-0.203463743702801,
-0.78555112003688));
#15870=CARTESIAN_POINT('Ctrl Pts',(-0.615966552324775,-0.224161999508995,
-0.763642258217233));
#15871=CARTESIAN_POINT('Ctrl Pts',(-0.631684198665438,-0.232861760990032,
-0.750785745543687));
#15872=CARTESIAN_POINT('Ctrl Pts',(-0.663382628119203,-0.244251601209411,
-0.722929908501543));
#15873=CARTESIAN_POINT('Ctrl Pts',(-0.679352081686668,-0.246942143572133,
-0.707917883896095));
#15874=CARTESIAN_POINT('Ctrl Pts',(-0.707917883896095,-0.246942143572133,
-0.679352081686668));
#15875=CARTESIAN_POINT('Ctrl Pts',(-0.722929908501543,-0.244251601209411,
-0.663382628119203));
#15876=CARTESIAN_POINT('Ctrl Pts',(-0.750785745543687,-0.232861760990032,
-0.631684198665439));
#15877=CARTESIAN_POINT('Ctrl Pts',(-0.763642258217232,-0.224161999508995,
-0.615966552324775));
#15878=CARTESIAN_POINT('Ctrl Pts',(-0.78555112003688,-0.203463743702801,
-0.587792702767295));
#15879=CARTESIAN_POINT('Ctrl Pts',(-0.795684265985088,-0.190326085855194,
-0.573915184558107));
#15880=CARTESIAN_POINT('Ctrl Pts',(-0.813159949759,-0.15976606450048,-0.548874290046456));
#15881=CARTESIAN_POINT('Ctrl Pts',(-0.820511285096538,-0.142345102874864,
-0.537715343527944));
#15882=CARTESIAN_POINT('Ctrl Pts',(-0.833661031856294,-0.0999305678883311,
-0.517157748491652));
#15883=CARTESIAN_POINT('Ctrl Pts',(-0.838633903678357,-0.0740444353928836,
-0.508899795931835));
#15884=CARTESIAN_POINT('Ctrl Pts',(-0.841298510752801,-0.04763,-0.504455939115715));
#15885=CARTESIAN_POINT('Origin',(-0.707106781186547,-0.04763,-0.707106781186548));
#15886=CARTESIAN_POINT('Origin',(0.,-0.04763,0.));
#15887=CARTESIAN_POINT('',(-0.238183666596899,-0.04763,-0.951592097314));
#15888=CARTESIAN_POINT('Origin',(0.,-0.04763,0.));
#15889=CARTESIAN_POINT('Origin',(5.55111512312578E-17,-0.04763,-1.));
#15890=CARTESIAN_POINT('Origin',(5.55111512312578E-17,0.,-1.));
#15891=CARTESIAN_POINT('',(0.238183666596899,-0.04763,-0.951592097314));
#15892=CARTESIAN_POINT('Ctrl Pts',(0.238183666596899,-0.04763,-0.951592097314));
#15893=CARTESIAN_POINT('Ctrl Pts',(0.233157223576062,-0.0740444353928835,
-0.952850216871763));
#15894=CARTESIAN_POINT('Ctrl Pts',(0.223801617934946,-0.099930567888331,
-0.955173119738174));
#15895=CARTESIAN_POINT('Ctrl Pts',(0.199966927975188,-0.142345102874864,
-0.960411259488514));
#15896=CARTESIAN_POINT('Ctrl Pts',(0.1868781821531,-0.15976606450048,-0.963103647174702));
#15897=CARTESIAN_POINT('Ctrl Pts',(0.15681442133453,-0.190326085855194,
-0.968453058988463));
#15898=CARTESIAN_POINT('Ctrl Pts',(0.139836317888042,-0.203463743702801,
-0.971100730005489));
#15899=CARTESIAN_POINT('Ctrl Pts',(0.104422493053067,-0.224161999508995,
-0.975530745318961));
#15900=CARTESIAN_POINT('Ctrl Pts',(0.0842175114474173,-0.232861760990032,
-0.977553872336861));
#15901=CARTESIAN_POINT('Ctrl Pts',(0.0421062857595698,-0.244251601209411,
-0.980270995488453));
#15902=CARTESIAN_POINT('Ctrl Pts',(0.0201990724523194,-0.246942143572133,
-0.980948));
#15903=CARTESIAN_POINT('Ctrl Pts',(-0.0201990724523193,-0.246942143572133,
-0.980948));
#15904=CARTESIAN_POINT('Ctrl Pts',(-0.0421062857595697,-0.244251601209411,
-0.980270995488453));
#15905=CARTESIAN_POINT('Ctrl Pts',(-0.0842175114474171,-0.232861760990032,
-0.977553872336861));
#15906=CARTESIAN_POINT('Ctrl Pts',(-0.104422493053067,-0.224161999508995,
-0.975530745318961));
#15907=CARTESIAN_POINT('Ctrl Pts',(-0.139836317888042,-0.203463743702801,
-0.971100730005489));
#15908=CARTESIAN_POINT('Ctrl Pts',(-0.15681442133453,-0.190326085855194,
-0.968453058988463));
#15909=CARTESIAN_POINT('Ctrl Pts',(-0.1868781821531,-0.15976606450048,-0.963103647174702));
#15910=CARTESIAN_POINT('Ctrl Pts',(-0.199966927975188,-0.142345102874864,
-0.960411259488514));
#15911=CARTESIAN_POINT('Ctrl Pts',(-0.223801617934945,-0.099930567888331,
-0.955173119738174));
#15912=CARTESIAN_POINT('Ctrl Pts',(-0.233157223576062,-0.0740444353928835,
-0.952850216871763));
#15913=CARTESIAN_POINT('Ctrl Pts',(-0.238183666596899,-0.0476299999999999,
-0.951592097314));
#15914=CARTESIAN_POINT('Origin',(5.55111512312578E-17,-0.04763,-1.));
#15915=CARTESIAN_POINT('Origin',(0.,-0.04763,0.));
#15916=CARTESIAN_POINT('',(0.504455939115715,-0.04763,-0.841298510752802));
#15917=CARTESIAN_POINT('Origin',(0.,-0.04763,0.));
#15918=CARTESIAN_POINT('Origin',(0.707106781186548,-0.04763,-0.707106781186547));
#15919=CARTESIAN_POINT('Origin',(0.707106781186548,0.,-0.707106781186547));
#15920=CARTESIAN_POINT('',(0.841298510752802,-0.04763,-0.504455939115715));
#15921=CARTESIAN_POINT('Ctrl Pts',(0.841298510752802,-0.04763,-0.504455939115715));
#15922=CARTESIAN_POINT('Ctrl Pts',(0.838633903678357,-0.0740444353928835,
-0.508899795931835));
#15923=CARTESIAN_POINT('Ctrl Pts',(0.833661031856294,-0.0999305678883309,
-0.517157748491652));
#15924=CARTESIAN_POINT('Ctrl Pts',(0.820511285096538,-0.142345102874864,
-0.537715343527944));
#15925=CARTESIAN_POINT('Ctrl Pts',(0.813159949759,-0.159766064500479,-0.548874290046456));
#15926=CARTESIAN_POINT('Ctrl Pts',(0.795684265985088,-0.190326085855194,
-0.573915184558107));
#15927=CARTESIAN_POINT('Ctrl Pts',(0.78555112003688,-0.203463743702801,
-0.587792702767295));
#15928=CARTESIAN_POINT('Ctrl Pts',(0.763642258217233,-0.224161999508995,
-0.615966552324775));
#15929=CARTESIAN_POINT('Ctrl Pts',(0.750785745543687,-0.232861760990032,
-0.631684198665438));
#15930=CARTESIAN_POINT('Ctrl Pts',(0.722929908501543,-0.244251601209411,
-0.663382628119203));
#15931=CARTESIAN_POINT('Ctrl Pts',(0.707917883896095,-0.246942143572133,
-0.679352081686668));
#15932=CARTESIAN_POINT('Ctrl Pts',(0.679352081686668,-0.246942143572133,
-0.707917883896095));
#15933=CARTESIAN_POINT('Ctrl Pts',(0.663382628119203,-0.244251601209411,
-0.722929908501543));
#15934=CARTESIAN_POINT('Ctrl Pts',(0.631684198665438,-0.232861760990032,
-0.750785745543687));
#15935=CARTESIAN_POINT('Ctrl Pts',(0.615966552324775,-0.224161999508995,
-0.763642258217232));
#15936=CARTESIAN_POINT('Ctrl Pts',(0.587792702767295,-0.203463743702801,
-0.78555112003688));
#15937=CARTESIAN_POINT('Ctrl Pts',(0.573915184558107,-0.190326085855194,
-0.795684265985088));
#15938=CARTESIAN_POINT('Ctrl Pts',(0.548874290046456,-0.159766064500479,
-0.813159949759));
#15939=CARTESIAN_POINT('Ctrl Pts',(0.537715343527944,-0.142345102874864,
-0.820511285096538));
#15940=CARTESIAN_POINT('Ctrl Pts',(0.517157748491652,-0.099930567888331,
-0.833661031856294));
#15941=CARTESIAN_POINT('Ctrl Pts',(0.508899795931835,-0.0740444353928835,
-0.838633903678357));
#15942=CARTESIAN_POINT('Ctrl Pts',(0.504455939115715,-0.04763,-0.841298510752801));
#15943=CARTESIAN_POINT('Origin',(0.707106781186548,-0.04763,-0.707106781186547));
#15944=CARTESIAN_POINT('Origin',(0.,-0.166705,0.));
#15945=CARTESIAN_POINT('',(-0.980948,-0.28578,1.20131482833E-16));
#15946=CARTESIAN_POINT('Origin',(0.,-0.28578,0.));
#15947=CARTESIAN_POINT('',(-0.980948,-0.166705,1.20131482833E-16));
#15948=CARTESIAN_POINT('',(0.951592097314,-0.04763,0.238183666596899));
#15949=CARTESIAN_POINT('Origin',(0.,-0.04763,0.));
#15950=CARTESIAN_POINT('',(0.951592097314,-0.04763,-0.238183666596899));
#15951=CARTESIAN_POINT('Ctrl Pts',(0.951592097314,-0.04763,0.238183666596899));
#15952=CARTESIAN_POINT('Ctrl Pts',(0.952850216871763,-0.0740444353928835,
0.233157223576062));
#15953=CARTESIAN_POINT('Ctrl Pts',(0.955173119738174,-0.099930567888331,
0.223801617934945));
#15954=CARTESIAN_POINT('Ctrl Pts',(0.960411259488514,-0.142345102874864,
0.199966927975188));
#15955=CARTESIAN_POINT('Ctrl Pts',(0.963103647174702,-0.15976606450048,
0.1868781821531));
#15956=CARTESIAN_POINT('Ctrl Pts',(0.968453058988463,-0.190326085855194,
0.15681442133453));
#15957=CARTESIAN_POINT('Ctrl Pts',(0.971100730005489,-0.203463743702801,
0.139836317888042));
#15958=CARTESIAN_POINT('Ctrl Pts',(0.975530745318961,-0.224161999508995,
0.104422493053067));
#15959=CARTESIAN_POINT('Ctrl Pts',(0.977553872336861,-0.232861760990032,
0.0842175114474172));
#15960=CARTESIAN_POINT('Ctrl Pts',(0.980270995488453,-0.244251601209411,
0.0421062857595697));
#15961=CARTESIAN_POINT('Ctrl Pts',(0.980948,-0.246942143572133,0.0201990724523194));
#15962=CARTESIAN_POINT('Ctrl Pts',(0.980948,-0.246942143572133,-0.0201990724523194));
#15963=CARTESIAN_POINT('Ctrl Pts',(0.980270995488453,-0.244251601209411,
-0.0421062857595697));
#15964=CARTESIAN_POINT('Ctrl Pts',(0.977553872336861,-0.232861760990032,
-0.0842175114474172));
#15965=CARTESIAN_POINT('Ctrl Pts',(0.975530745318961,-0.224161999508995,
-0.104422493053067));
#15966=CARTESIAN_POINT('Ctrl Pts',(0.971100730005489,-0.203463743702801,
-0.139836317888042));
#15967=CARTESIAN_POINT('Ctrl Pts',(0.968453058988463,-0.190326085855194,
-0.15681442133453));
#15968=CARTESIAN_POINT('Ctrl Pts',(0.963103647174702,-0.15976606450048,
-0.1868781821531));
#15969=CARTESIAN_POINT('Ctrl Pts',(0.960411259488514,-0.142345102874864,
-0.199966927975188));
#15970=CARTESIAN_POINT('Ctrl Pts',(0.955173119738174,-0.099930567888331,
-0.223801617934945));
#15971=CARTESIAN_POINT('Ctrl Pts',(0.952850216871763,-0.0740444353928835,
-0.233157223576062));
#15972=CARTESIAN_POINT('Ctrl Pts',(0.951592097314,-0.0476299999999999,-0.238183666596899));
#15973=CARTESIAN_POINT('Origin',(0.,-0.04763,0.));
#15974=CARTESIAN_POINT('Origin',(0.,-0.04763,0.));
#15975=CARTESIAN_POINT('Origin',(1.,-0.04763,0.));
#15976=CARTESIAN_POINT('Origin',(1.,0.,0.));
#15977=CARTESIAN_POINT('Origin',(1.,-0.04763,0.));
#15978=CARTESIAN_POINT('Origin',(0.,-0.28578,0.));
#15979=CARTESIAN_POINT('Origin',(0.,-0.04763,0.));
#15980=CARTESIAN_POINT('',(0.,0.,0.));
#15981=CARTESIAN_POINT('Origin',(1.013815,0.445,0.));
#15982=CARTESIAN_POINT('',(-1.013815,0.445,-1.24156529467757E-16));
#15983=CARTESIAN_POINT('Origin',(0.,0.445,0.));
#15984=CARTESIAN_POINT('',(-0.991185,0.445,-1.21385153761287E-16));
#15985=CARTESIAN_POINT('Origin',(0.,0.445,0.));
#15986=CARTESIAN_POINT('Origin',(0.,0.4075,0.));
#15987=CARTESIAN_POINT('',(-1.013815,0.37,-1.24156529467757E-16));
#15988=CARTESIAN_POINT('Origin',(0.,0.37,0.));
#15989=CARTESIAN_POINT('',(-1.013815,0.4075,-1.24156529467757E-16));
#15990=CARTESIAN_POINT('Origin',(0.991185,0.37,0.));
#15991=CARTESIAN_POINT('',(-0.991185,0.37,-1.21385153761287E-16));
#15992=CARTESIAN_POINT('Origin',(0.,0.37,0.));
#15993=CARTESIAN_POINT('Origin',(0.,0.4075,0.));
#15994=CARTESIAN_POINT('',(-0.991185,0.4075,-1.21385153761287E-16));
#15995=CARTESIAN_POINT('Origin',(1.013815,-0.37,0.));
#15996=CARTESIAN_POINT('',(-1.013815,-0.37,-1.24156529467757E-16));
#15997=CARTESIAN_POINT('Origin',(0.,-0.37,0.));
#15998=CARTESIAN_POINT('',(-0.991185,-0.37,-1.21385153761287E-16));
#15999=CARTESIAN_POINT('Origin',(0.,-0.37,0.));
#16000=CARTESIAN_POINT('Origin',(0.,-0.4075,0.));
#16001=CARTESIAN_POINT('',(-1.013815,-0.445,-1.24156529467757E-16));
#16002=CARTESIAN_POINT('Origin',(0.,-0.445,0.));
#16003=CARTESIAN_POINT('',(-1.013815,-0.4075,-1.24156529467757E-16));
#16004=CARTESIAN_POINT('Origin',(0.991185,-0.445,0.));
#16005=CARTESIAN_POINT('',(-0.991185,-0.445,-1.21385153761287E-16));
#16006=CARTESIAN_POINT('Origin',(0.,-0.445,0.));
#16007=CARTESIAN_POINT('Origin',(0.,-0.4075,0.));
#16008=CARTESIAN_POINT('',(-0.991185,-0.4075,-1.21385153761287E-16));
#16009=CARTESIAN_POINT('',(0.,0.,0.));
#16010=CARTESIAN_POINT('',(0.,0.,0.));
#16011=CARTESIAN_POINT('',(0.,0.,0.));
#16012=CARTESIAN_POINT('',(0.,0.,0.));
#16013=CARTESIAN_POINT('',(0.,0.,0.));
#16014=CARTESIAN_POINT('',(0.,0.,0.));
#16015=CARTESIAN_POINT('',(0.,0.,0.));
#16016=CARTESIAN_POINT('',(0.,0.,0.));
#16017=CARTESIAN_POINT('',(0.,0.,0.));
#16018=CARTESIAN_POINT('',(0.,0.,0.));
#16019=CARTESIAN_POINT('',(1.,3.95,12.));
#16020=CARTESIAN_POINT('',(11.,3.95,12.));
#16021=CARTESIAN_POINT('',(0.,0.,0.));
#16022=CARTESIAN_POINT('',(0.,0.,0.));
#16023=CARTESIAN_POINT('Origin',(11.,-3.2,6.9));
#16024=CARTESIAN_POINT('',(10.79,-3.2,6.9));
#16025=CARTESIAN_POINT('Origin',(11.,-3.2,6.9));
#16026=CARTESIAN_POINT('',(10.79,-3.2,8.));
#16027=CARTESIAN_POINT('',(10.79,-3.2,6.9));
#16028=CARTESIAN_POINT('Origin',(11.,-3.2,8.));
#16029=CARTESIAN_POINT('Origin',(11.,-3.2,6.9));
#16030=CARTESIAN_POINT('Origin',(11.,0.2,6.9));
#16031=CARTESIAN_POINT('',(10.79,0.2,6.9));
#16032=CARTESIAN_POINT('Origin',(11.,0.2,6.9));
#16033=CARTESIAN_POINT('',(10.79,0.2,8.));
#16034=CARTESIAN_POINT('',(10.79,0.2,6.9));
#16035=CARTESIAN_POINT('Origin',(11.,0.2,8.));
#16036=CARTESIAN_POINT('Origin',(11.,0.2,6.9));
#16037=CARTESIAN_POINT('Origin',(10.,-4.,7.5));
#16038=CARTESIAN_POINT('',(10.,-4.,8.));
#16039=CARTESIAN_POINT('',(10.,-4.,7.5));
#16040=CARTESIAN_POINT('',(10.,-4.,8.));
#16041=CARTESIAN_POINT('',(10.,1.,8.));
#16042=CARTESIAN_POINT('',(10.,-4.,8.));
#16043=CARTESIAN_POINT('',(10.,1.,7.5));
#16044=CARTESIAN_POINT('',(10.,1.,8.));
#16045=CARTESIAN_POINT('',(10.,-2.,7.5));
#16046=CARTESIAN_POINT('Origin',(12.,-4.,8.));
#16047=CARTESIAN_POINT('',(12.,-4.,7.5));
#16048=CARTESIAN_POINT('',(12.,-4.,8.));
#16049=CARTESIAN_POINT('',(12.,-4.,7.5));
#16050=CARTESIAN_POINT('',(12.,1.,7.5));
#16051=CARTESIAN_POINT('',(12.,-2.,7.5));
#16052=CARTESIAN_POINT('',(12.,1.,8.));
#16053=CARTESIAN_POINT('',(12.,1.,7.5));
#16054=CARTESIAN_POINT('',(12.,-4.,8.));
#16055=CARTESIAN_POINT('Origin',(10.,-4.,8.));
#16056=CARTESIAN_POINT('',(12.,-4.,8.));
#16057=CARTESIAN_POINT('',(12.,1.,8.));
#16058=CARTESIAN_POINT('Origin',(11.,1.,7.75));
#16059=CARTESIAN_POINT('',(11.,1.,7.5));
#16060=CARTESIAN_POINT('Origin',(11.,2.7,12.));
#16061=CARTESIAN_POINT('',(10.5,2.8,12.));
#16062=CARTESIAN_POINT('Origin',(11.,2.8,12.));
#16063=CARTESIAN_POINT('',(10.5,3.3,12.));
#16064=CARTESIAN_POINT('',(10.5,2.7,12.));
#16065=CARTESIAN_POINT('Origin',(11.,3.3,12.));
#16066=CARTESIAN_POINT('Origin',(11.,2.8,10.15));
#16067=CARTESIAN_POINT('',(12.,2.8,7.5));
#16068=CARTESIAN_POINT('',(10.,2.8,7.5));
#16069=CARTESIAN_POINT('',(11.,2.8,7.5));
#16070=CARTESIAN_POINT('',(12.,2.8,13.));
#16071=CARTESIAN_POINT('',(12.,2.8,7.3));
#16072=CARTESIAN_POINT('',(10.,2.8,13.));
#16073=CARTESIAN_POINT('',(12.,2.8,13.));
#16074=CARTESIAN_POINT('',(10.,2.8,13.));
#16075=CARTESIAN_POINT('Origin',(12.,2.8,13.));
#16076=CARTESIAN_POINT('',(12.,3.3,7.5));
#16077=CARTESIAN_POINT('',(12.,1.4,7.5));
#16078=CARTESIAN_POINT('',(12.,3.3,13.));
#16079=CARTESIAN_POINT('',(12.,3.3,7.3));
#16080=CARTESIAN_POINT('',(12.,2.8,13.));
#16081=CARTESIAN_POINT('Origin',(10.,2.8,7.3));
#16082=CARTESIAN_POINT('',(10.,3.3,7.5));
#16083=CARTESIAN_POINT('',(10.,1.4,7.5));
#16084=CARTESIAN_POINT('',(10.,3.3,13.));
#16085=CARTESIAN_POINT('',(10.,2.8,13.));
#16086=CARTESIAN_POINT('',(10.,3.3,13.));
#16087=CARTESIAN_POINT('Origin',(10.,2.8,13.));
#16088=CARTESIAN_POINT('',(12.,3.3,13.));
#16089=CARTESIAN_POINT('Origin',(11.,3.3,10.15));
#16090=CARTESIAN_POINT('',(11.,3.3,7.5));
#16091=CARTESIAN_POINT('Origin',(12.5,-1.9,6.6));
#16092=CARTESIAN_POINT('',(12.225,-1.9,6.7));
#16093=CARTESIAN_POINT('Origin',(12.5,-1.9,6.7));
#16094=CARTESIAN_POINT('',(12.225,-1.9,7.5));
#16095=CARTESIAN_POINT('',(12.225,-1.9,6.6));
#16096=CARTESIAN_POINT('Origin',(12.5,-1.9,7.5));
#16097=CARTESIAN_POINT('Origin',(9.5,1.9,6.6));
#16098=CARTESIAN_POINT('',(9.225,1.9,6.7));
#16099=CARTESIAN_POINT('Origin',(9.5,1.9,6.7));
#16100=CARTESIAN_POINT('',(9.225,1.9,7.5));
#16101=CARTESIAN_POINT('',(9.225,1.9,6.6));
#16102=CARTESIAN_POINT('Origin',(9.5,1.9,7.5));
#16103=CARTESIAN_POINT('Origin',(9.5,-1.9,6.6));
#16104=CARTESIAN_POINT('',(9.225,-1.9,6.7));
#16105=CARTESIAN_POINT('Origin',(9.5,-1.9,6.7));
#16106=CARTESIAN_POINT('',(9.225,-1.9,7.5));
#16107=CARTESIAN_POINT('',(9.225,-1.9,6.6));
#16108=CARTESIAN_POINT('Origin',(9.5,-1.9,7.5));
#16109=CARTESIAN_POINT('Origin',(12.5,1.9,6.6));
#16110=CARTESIAN_POINT('',(12.225,1.9,6.7));
#16111=CARTESIAN_POINT('Origin',(12.5,1.9,6.7));
#16112=CARTESIAN_POINT('',(12.225,1.9,7.5));
#16113=CARTESIAN_POINT('',(12.225,1.9,6.6));
#16114=CARTESIAN_POINT('Origin',(12.5,1.9,7.5));
#16115=CARTESIAN_POINT('Origin',(15.,4.,6.7));
#16116=CARTESIAN_POINT('',(15.,4.,6.7));
#16117=CARTESIAN_POINT('',(7.,4.,6.7));
#16118=CARTESIAN_POINT('',(15.,4.,6.7));
#16119=CARTESIAN_POINT('',(7.,4.,7.5));
#16120=CARTESIAN_POINT('',(7.,4.,6.7));
#16121=CARTESIAN_POINT('',(15.,4.,7.5));
#16122=CARTESIAN_POINT('',(15.,4.,7.5));
#16123=CARTESIAN_POINT('',(15.,4.,6.7));
#16124=CARTESIAN_POINT('Origin',(15.,-4.,6.7));
#16125=CARTESIAN_POINT('',(15.,-4.,6.7));
#16126=CARTESIAN_POINT('',(15.,-4.,6.7));
#16127=CARTESIAN_POINT('',(15.,-4.,7.5));
#16128=CARTESIAN_POINT('',(15.,-4.,7.5));
#16129=CARTESIAN_POINT('',(15.,-4.,6.7));
#16130=CARTESIAN_POINT('Origin',(7.,-4.,6.7));
#16131=CARTESIAN_POINT('',(7.,-4.,6.7));
#16132=CARTESIAN_POINT('',(7.,-4.,6.7));
#16133=CARTESIAN_POINT('',(7.,-4.,7.5));
#16134=CARTESIAN_POINT('',(7.,-4.,7.5));
#16135=CARTESIAN_POINT('',(7.,-4.,7.5));
#16136=CARTESIAN_POINT('',(7.,-4.,6.7));
#16137=CARTESIAN_POINT('Origin',(7.,4.,6.7));
#16138=CARTESIAN_POINT('',(7.,4.,6.7));
#16139=CARTESIAN_POINT('',(7.,4.,7.5));
#16140=CARTESIAN_POINT('Origin',(11.,0.,7.5));
#16141=CARTESIAN_POINT('Origin',(11.,0.,6.7));
#16142=CARTESIAN_POINT('',(0.,0.,0.));
#16143=CARTESIAN_POINT('Origin',(11.,-3.2,8.9));
#16144=CARTESIAN_POINT('',(10.725,-3.2,9.));
#16145=CARTESIAN_POINT('Origin',(11.,-3.2,9.));
#16146=CARTESIAN_POINT('',(10.725,-3.2,9.5));
#16147=CARTESIAN_POINT('',(10.725,-3.2,8.9));
#16148=CARTESIAN_POINT('Origin',(11.,-3.2,9.5));
#16149=CARTESIAN_POINT('Origin',(11.,0.2,8.9));
#16150=CARTESIAN_POINT('',(10.725,0.2,9.));
#16151=CARTESIAN_POINT('Origin',(11.,0.2,9.));
#16152=CARTESIAN_POINT('',(10.725,0.2,9.5));
#16153=CARTESIAN_POINT('',(10.725,0.2,8.9));
#16154=CARTESIAN_POINT('Origin',(11.,0.2,9.5));
#16155=CARTESIAN_POINT('Origin',(12.,1.,9.));
#16156=CARTESIAN_POINT('',(12.,1.,9.));
#16157=CARTESIAN_POINT('',(10.,1.,9.));
#16158=CARTESIAN_POINT('',(12.,1.,9.));
#16159=CARTESIAN_POINT('',(10.,1.,9.5));
#16160=CARTESIAN_POINT('',(10.,1.,9.));
#16161=CARTESIAN_POINT('',(12.,1.,9.5));
#16162=CARTESIAN_POINT('',(12.,1.,9.5));
#16163=CARTESIAN_POINT('',(12.,1.,9.));
#16164=CARTESIAN_POINT('Origin',(12.,-4.,9.));
#16165=CARTESIAN_POINT('',(12.,-4.,9.));
#16166=CARTESIAN_POINT('',(12.,-4.,9.));
#16167=CARTESIAN_POINT('',(12.,-4.,9.5));
#16168=CARTESIAN_POINT('',(12.,-4.,9.5));
#16169=CARTESIAN_POINT('',(12.,-4.,9.));
#16170=CARTESIAN_POINT('Origin',(10.,-4.,9.));
#16171=CARTESIAN_POINT('',(10.,-4.,9.));
#16172=CARTESIAN_POINT('',(10.,-4.,9.));
#16173=CARTESIAN_POINT('',(10.,-4.,9.5));
#16174=CARTESIAN_POINT('',(10.,-4.,9.5));
#16175=CARTESIAN_POINT('',(10.,-4.,9.));
#16176=CARTESIAN_POINT('Origin',(10.,1.,9.));
#16177=CARTESIAN_POINT('',(10.,1.,9.));
#16178=CARTESIAN_POINT('',(10.,1.,9.5));
#16179=CARTESIAN_POINT('Origin',(11.,-1.5,9.5));
#16180=CARTESIAN_POINT('Origin',(11.,-1.5,9.));
#16181=CARTESIAN_POINT('',(0.,0.,0.));
#16182=CARTESIAN_POINT('Origin',(11.,3.7,12.));
#16183=CARTESIAN_POINT('',(10.835,3.7,12.));
#16184=CARTESIAN_POINT('Origin',(11.,3.7,12.));
#16185=CARTESIAN_POINT('',(10.835,4.8,12.));
#16186=CARTESIAN_POINT('',(10.835,3.7,12.));
#16187=CARTESIAN_POINT('Origin',(11.,4.8,12.));
#16188=CARTESIAN_POINT('Origin',(11.,3.7,12.));
#16189=CARTESIAN_POINT('Origin',(11.,2.8,12.));
#16190=CARTESIAN_POINT('',(10.2,2.8,12.));
#16191=CARTESIAN_POINT('Origin',(11.,2.8,12.));
#16192=CARTESIAN_POINT('',(10.5,2.8,12.));
#16193=CARTESIAN_POINT('Origin',(11.,2.8,12.));
#16194=CARTESIAN_POINT('Origin',(11.,2.4,12.));
#16195=CARTESIAN_POINT('',(10.2,2.4,12.));
#16196=CARTESIAN_POINT('',(10.2,2.4,12.));
#16197=CARTESIAN_POINT('Origin',(11.,2.4,12.));
#16198=CARTESIAN_POINT('Origin',(11.,2.4,12.));
#16199=CARTESIAN_POINT('Origin',(11.,2.8,12.));
#16200=CARTESIAN_POINT('',(10.5,4.8,12.));
#16201=CARTESIAN_POINT('Origin',(11.,4.8,12.));
#16202=CARTESIAN_POINT('',(10.5,2.8,12.));
#16203=CARTESIAN_POINT('Origin',(11.,4.8,12.));
#16204=CARTESIAN_POINT('',(0.,0.,0.));
#16205=CARTESIAN_POINT('Origin',(11.,3.3,12.));
#16206=CARTESIAN_POINT('',(10.495,3.5,12.));
#16207=CARTESIAN_POINT('Origin',(11.,3.5,12.));
#16208=CARTESIAN_POINT('',(10.495,3.3,12.));
#16209=CARTESIAN_POINT('',(10.495,3.3,12.));
#16210=CARTESIAN_POINT('Origin',(11.,3.3,12.));
#16211=CARTESIAN_POINT('Origin',(11.,3.3,12.));
#16212=CARTESIAN_POINT('',(10.3,3.5,12.));
#16213=CARTESIAN_POINT('Origin',(11.,3.5,12.));
#16214=CARTESIAN_POINT('',(10.3,3.3,12.));
#16215=CARTESIAN_POINT('',(10.3,3.3,12.));
#16216=CARTESIAN_POINT('Origin',(11.,3.3,12.));
#16217=CARTESIAN_POINT('Origin',(11.,3.5,12.));
#16218=CARTESIAN_POINT('Origin',(11.,3.3,12.));
#16219=CARTESIAN_POINT('',(0.,0.,0.));
#16220=CARTESIAN_POINT('Origin',(11.,4.4,12.));
#16221=CARTESIAN_POINT('',(10.495,4.8,12.));
#16222=CARTESIAN_POINT('Origin',(11.,4.8,12.));
#16223=CARTESIAN_POINT('',(10.495,4.4,12.));
#16224=CARTESIAN_POINT('',(10.495,4.4,12.));
#16225=CARTESIAN_POINT('Origin',(11.,4.4,12.));
#16226=CARTESIAN_POINT('Origin',(11.,4.4,12.));
#16227=CARTESIAN_POINT('',(10.3,4.8,12.));
#16228=CARTESIAN_POINT('Origin',(11.,4.8,12.));
#16229=CARTESIAN_POINT('',(10.3,4.4,12.));
#16230=CARTESIAN_POINT('',(10.3,4.4,12.));
#16231=CARTESIAN_POINT('Origin',(11.,4.4,12.));
#16232=CARTESIAN_POINT('Origin',(11.,4.8,12.));
#16233=CARTESIAN_POINT('Origin',(11.,4.4,12.));
#16234=CARTESIAN_POINT('',(0.,0.,0.));
#16235=CARTESIAN_POINT('Origin',(11.,4.8,12.));
#16236=CARTESIAN_POINT('',(10.775,5.,12.));
#16237=CARTESIAN_POINT('Origin',(11.,5.,12.));
#16238=CARTESIAN_POINT('',(10.775,4.8,12.));
#16239=CARTESIAN_POINT('',(10.775,4.8,12.));
#16240=CARTESIAN_POINT('Origin',(11.,4.8,12.));
#16241=CARTESIAN_POINT('Origin',(11.,4.8,12.));
#16242=CARTESIAN_POINT('',(10.2,5.,12.));
#16243=CARTESIAN_POINT('Origin',(11.,5.,12.));
#16244=CARTESIAN_POINT('',(10.2,4.8,12.));
#16245=CARTESIAN_POINT('',(10.2,4.8,12.));
#16246=CARTESIAN_POINT('Origin',(11.,4.8,12.));
#16247=CARTESIAN_POINT('Origin',(11.,5.,12.));
#16248=CARTESIAN_POINT('Origin',(11.,4.8,12.));
#16249=CARTESIAN_POINT('',(0.,0.,0.));
#16250=CARTESIAN_POINT('',(0.,0.,0.));
#16251=CARTESIAN_POINT('Origin',(1.5,-1.9,1.7));
#16252=CARTESIAN_POINT('',(1.56403124237433,-1.7,1.7));
#16253=CARTESIAN_POINT('',(1.43596875762567,-1.7,1.7));
#16254=CARTESIAN_POINT('',(0.75,-1.7,1.7));
#16255=CARTESIAN_POINT('Origin',(1.5,-1.9,1.7));
#16256=CARTESIAN_POINT('Origin',(1.5,-1.9,1.7));
#16257=CARTESIAN_POINT('',(1.56403124237433,-1.7,1.75));
#16258=CARTESIAN_POINT('',(1.56403124237433,-1.7,1.7));
#16259=CARTESIAN_POINT('',(1.29,-1.9,1.75));
#16260=CARTESIAN_POINT('Origin',(1.5,-1.9,1.75));
#16261=CARTESIAN_POINT('',(1.29,-1.9,2.4));
#16262=CARTESIAN_POINT('',(1.29,-1.9,1.7));
#16263=CARTESIAN_POINT('Origin',(1.5,-1.9,2.4));
#16264=CARTESIAN_POINT('',(1.43596875762567,-1.7,1.75));
#16265=CARTESIAN_POINT('Origin',(1.5,-1.9,1.75));
#16266=CARTESIAN_POINT('',(1.43596875762567,-1.7,1.7));
#16267=CARTESIAN_POINT('Origin',(-1.5,1.9,1.7));
#16268=CARTESIAN_POINT('',(-1.56403124237433,1.7,1.7));
#16269=CARTESIAN_POINT('',(-1.43596875762567,1.7,1.7));
#16270=CARTESIAN_POINT('',(-0.75,1.7,1.7));
#16271=CARTESIAN_POINT('Origin',(-1.5,1.9,1.7));
#16272=CARTESIAN_POINT('Origin',(-1.5,1.9,1.7));
#16273=CARTESIAN_POINT('',(-1.56403124237433,1.7,1.75));
#16274=CARTESIAN_POINT('',(-1.56403124237433,1.7,1.7));
#16275=CARTESIAN_POINT('',(-1.71,1.9,1.75));
#16276=CARTESIAN_POINT('Origin',(-1.5,1.9,1.75));
#16277=CARTESIAN_POINT('',(-1.71,1.9,2.4));
#16278=CARTESIAN_POINT('',(-1.71,1.9,1.7));
#16279=CARTESIAN_POINT('Origin',(-1.5,1.9,2.4));
#16280=CARTESIAN_POINT('',(-1.43596875762567,1.7,1.75));
#16281=CARTESIAN_POINT('Origin',(-1.5,1.9,1.75));
#16282=CARTESIAN_POINT('',(-1.43596875762567,1.7,1.7));
#16283=CARTESIAN_POINT('Origin',(-1.5,-1.9,1.7));
#16284=CARTESIAN_POINT('',(-1.43596875762567,-1.7,1.7));
#16285=CARTESIAN_POINT('',(-1.56403124237433,-1.7,1.7));
#16286=CARTESIAN_POINT('',(-0.75,-1.7,1.7));
#16287=CARTESIAN_POINT('Origin',(-1.5,-1.9,1.7));
#16288=CARTESIAN_POINT('Origin',(-1.5,-1.9,1.7));
#16289=CARTESIAN_POINT('',(-1.43596875762567,-1.7,1.75));
#16290=CARTESIAN_POINT('',(-1.43596875762567,-1.7,1.7));
#16291=CARTESIAN_POINT('',(-1.71,-1.9,1.75));
#16292=CARTESIAN_POINT('Origin',(-1.5,-1.9,1.75));
#16293=CARTESIAN_POINT('',(-1.71,-1.9,2.4));
#16294=CARTESIAN_POINT('',(-1.71,-1.9,1.7));
#16295=CARTESIAN_POINT('Origin',(-1.5,-1.9,2.4));
#16296=CARTESIAN_POINT('',(-1.56403124237433,-1.7,1.75));
#16297=CARTESIAN_POINT('Origin',(-1.5,-1.9,1.75));
#16298=CARTESIAN_POINT('',(-1.56403124237433,-1.7,1.7));
#16299=CARTESIAN_POINT('Origin',(1.5,1.9,1.7));
#16300=CARTESIAN_POINT('',(1.43596875762567,1.7,1.7));
#16301=CARTESIAN_POINT('',(1.56403124237433,1.7,1.7));
#16302=CARTESIAN_POINT('',(0.75,1.7,1.7));
#16303=CARTESIAN_POINT('Origin',(1.5,1.9,1.7));
#16304=CARTESIAN_POINT('Origin',(1.5,1.9,1.7));
#16305=CARTESIAN_POINT('',(1.43596875762567,1.7,1.75));
#16306=CARTESIAN_POINT('',(1.43596875762567,1.7,1.7));
#16307=CARTESIAN_POINT('',(1.29,1.9,1.75));
#16308=CARTESIAN_POINT('Origin',(1.5,1.9,1.75));
#16309=CARTESIAN_POINT('',(1.29,1.9,2.4));
#16310=CARTESIAN_POINT('',(1.29,1.9,1.7));
#16311=CARTESIAN_POINT('Origin',(1.5,1.9,2.4));
#16312=CARTESIAN_POINT('',(1.56403124237433,1.7,1.75));
#16313=CARTESIAN_POINT('Origin',(1.5,1.9,1.75));
#16314=CARTESIAN_POINT('',(1.56403124237433,1.7,1.7));
#16315=CARTESIAN_POINT('Origin',(0.,-1.7,1.75));
#16316=CARTESIAN_POINT('',(0.,-1.7,1.75));
#16317=CARTESIAN_POINT('',(-1.97,-1.7,1.75));
#16318=CARTESIAN_POINT('',(0.,-1.7,1.75));
#16319=CARTESIAN_POINT('',(-1.97,-1.7,0.43));
#16320=CARTESIAN_POINT('',(-1.97,-1.7,1.75));
#16321=CARTESIAN_POINT('',(1.97,-1.7,0.43));
#16322=CARTESIAN_POINT('',(0.,-1.7,0.43));
#16323=CARTESIAN_POINT('',(1.97,-1.7,1.75));
#16324=CARTESIAN_POINT('',(1.97,-1.7,1.75));
#16325=CARTESIAN_POINT('',(0.,-1.7,1.75));
#16326=CARTESIAN_POINT('Origin',(0.,1.7,0.43));
#16327=CARTESIAN_POINT('',(0.,1.7,1.75));
#16328=CARTESIAN_POINT('',(1.97,1.7,1.75));
#16329=CARTESIAN_POINT('',(0.,1.7,1.75));
#16330=CARTESIAN_POINT('',(1.97,1.7,0.43));
#16331=CARTESIAN_POINT('',(1.97,1.7,0.43));
#16332=CARTESIAN_POINT('',(-1.97,1.7,0.43));
#16333=CARTESIAN_POINT('',(0.,1.7,0.43));
#16334=CARTESIAN_POINT('',(-1.97,1.7,1.75));
#16335=CARTESIAN_POINT('',(-1.97,1.7,0.43));
#16336=CARTESIAN_POINT('',(0.,1.7,1.75));
#16337=CARTESIAN_POINT('Origin',(-1.97,0.,1.415));
#16338=CARTESIAN_POINT('',(-1.97,-2.35,1.75));
#16339=CARTESIAN_POINT('',(-1.97,-2.35,1.75));
#16340=CARTESIAN_POINT('',(-1.97,-2.35,2.4));
#16341=CARTESIAN_POINT('',(-1.97,-2.35,2.4));
#16342=CARTESIAN_POINT('',(-1.97,2.35,2.4));
#16343=CARTESIAN_POINT('',(-1.97,2.35,2.4));
#16344=CARTESIAN_POINT('',(-1.97,2.35,1.75));
#16345=CARTESIAN_POINT('',(-1.97,2.35,1.75));
#16346=CARTESIAN_POINT('',(-1.97,1.7,1.75));
#16347=CARTESIAN_POINT('',(-1.97,0.78,0.43));
#16348=CARTESIAN_POINT('',(-1.97,0.78,0.43));
#16349=CARTESIAN_POINT('',(-1.97,0.78,1.55));
#16350=CARTESIAN_POINT('',(-1.97,0.78,1.55));
#16351=CARTESIAN_POINT('',(-1.97,-0.78,1.55));
#16352=CARTESIAN_POINT('',(-1.97,-0.78,1.55));
#16353=CARTESIAN_POINT('',(-1.97,-0.78,0.43));
#16354=CARTESIAN_POINT('',(-1.97,-0.78,0.43));
#16355=CARTESIAN_POINT('',(-1.97,-1.7,0.43));
#16356=CARTESIAN_POINT('Origin',(0.,-2.35,1.75));
#16357=CARTESIAN_POINT('',(1.97,-2.35,1.75));
#16358=CARTESIAN_POINT('',(1.97,-2.35,1.75));
#16359=CARTESIAN_POINT('',(0.,-2.35,1.75));
#16360=CARTESIAN_POINT('Origin',(0.,-2.35,2.4));
#16361=CARTESIAN_POINT('',(1.97,-2.35,2.4));
#16362=CARTESIAN_POINT('',(1.97,-2.35,2.4));
#16363=CARTESIAN_POINT('',(0.,-2.35,2.4));
#16364=CARTESIAN_POINT('Origin',(0.,2.35,2.4));
#16365=CARTESIAN_POINT('',(1.97,2.35,2.4));
#16366=CARTESIAN_POINT('',(1.97,2.35,2.4));
#16367=CARTESIAN_POINT('',(0.,2.35,2.4));
#16368=CARTESIAN_POINT('Origin',(0.,2.35,1.75));
#16369=CARTESIAN_POINT('',(1.97,2.35,1.75));
#16370=CARTESIAN_POINT('',(1.97,2.35,1.75));
#16371=CARTESIAN_POINT('',(0.,2.35,1.75));
#16372=CARTESIAN_POINT('Origin',(0.,1.7,1.75));
#16373=CARTESIAN_POINT('',(1.97,1.7,1.75));
#16374=CARTESIAN_POINT('Origin',(0.,0.78,0.43));
#16375=CARTESIAN_POINT('',(1.97,0.78,0.43));
#16376=CARTESIAN_POINT('',(1.97,0.78,0.43));
#16377=CARTESIAN_POINT('',(0.,0.78,0.43));
#16378=CARTESIAN_POINT('Origin',(0.,0.78,1.55));
#16379=CARTESIAN_POINT('',(1.97,0.78,1.55));
#16380=CARTESIAN_POINT('',(1.97,0.78,1.55));
#16381=CARTESIAN_POINT('',(0.,0.78,1.55));
#16382=CARTESIAN_POINT('Origin',(0.,-0.78,1.55));
#16383=CARTESIAN_POINT('',(1.97,-0.78,1.55));
#16384=CARTESIAN_POINT('',(1.97,-0.78,1.55));
#16385=CARTESIAN_POINT('',(0.,-0.78,1.55));
#16386=CARTESIAN_POINT('Origin',(0.,-0.78,0.43));
#16387=CARTESIAN_POINT('',(1.97,-0.78,0.43));
#16388=CARTESIAN_POINT('',(1.97,-0.78,0.43));
#16389=CARTESIAN_POINT('',(0.,-0.78,0.43));
#16390=CARTESIAN_POINT('Origin',(0.,-1.7,0.43));
#16391=CARTESIAN_POINT('',(1.97,-1.7,0.43));
#16392=CARTESIAN_POINT('Origin',(1.97,0.,1.415));
#16393=CARTESIAN_POINT('',(0.,0.,0.));
#16394=CARTESIAN_POINT('Origin',(1.97,1.7,2.3));
#16395=CARTESIAN_POINT('',(1.97,1.7,2.3));
#16396=CARTESIAN_POINT('',(1.97,-1.7,2.3));
#16397=CARTESIAN_POINT('',(1.97,1.7,2.3));
#16398=CARTESIAN_POINT('',(3.07,-1.7,2.3));
#16399=CARTESIAN_POINT('',(1.97,-1.7,2.3));
#16400=CARTESIAN_POINT('',(3.07,1.7,2.3));
#16401=CARTESIAN_POINT('',(3.07,1.7,2.3));
#16402=CARTESIAN_POINT('',(1.97,1.7,2.3));
#16403=CARTESIAN_POINT('Origin',(1.97,1.7,0.46));
#16404=CARTESIAN_POINT('',(1.97,1.7,0.46));
#16405=CARTESIAN_POINT('',(1.97,1.7,0.46));
#16406=CARTESIAN_POINT('',(3.07,1.7,0.46));
#16407=CARTESIAN_POINT('',(3.07,1.7,0.46));
#16408=CARTESIAN_POINT('',(1.97,1.7,0.46));
#16409=CARTESIAN_POINT('Origin',(1.97,0.78,0.46));
#16410=CARTESIAN_POINT('',(1.97,0.78,0.46));
#16411=CARTESIAN_POINT('',(1.97,0.78,0.46));
#16412=CARTESIAN_POINT('',(3.07,0.78,0.46));
#16413=CARTESIAN_POINT('',(3.07,0.78,0.46));
#16414=CARTESIAN_POINT('',(1.97,0.78,0.46));
#16415=CARTESIAN_POINT('Origin',(1.97,0.78,1.55));
#16416=CARTESIAN_POINT('',(1.97,0.78,1.55));
#16417=CARTESIAN_POINT('',(1.97,0.78,1.55));
#16418=CARTESIAN_POINT('',(3.07,0.78,1.55));
#16419=CARTESIAN_POINT('',(3.07,0.78,1.55));
#16420=CARTESIAN_POINT('',(1.97,0.78,1.55));
#16421=CARTESIAN_POINT('Origin',(1.97,-0.78,1.55));
#16422=CARTESIAN_POINT('',(1.97,-0.78,1.55));
#16423=CARTESIAN_POINT('',(1.97,-0.78,1.55));
#16424=CARTESIAN_POINT('',(3.07,-0.78,1.55));
#16425=CARTESIAN_POINT('',(3.07,-0.78,1.55));
#16426=CARTESIAN_POINT('',(1.97,-0.78,1.55));
#16427=CARTESIAN_POINT('Origin',(1.97,-0.78,0.46));
#16428=CARTESIAN_POINT('',(1.97,-0.78,0.46));
#16429=CARTESIAN_POINT('',(1.97,-0.78,0.46));
#16430=CARTESIAN_POINT('',(3.07,-0.78,0.46));
#16431=CARTESIAN_POINT('',(3.07,-0.78,0.46));
#16432=CARTESIAN_POINT('',(1.97,-0.78,0.46));
#16433=CARTESIAN_POINT('Origin',(1.97,-1.7,0.46));
#16434=CARTESIAN_POINT('',(1.97,-1.7,0.46));
#16435=CARTESIAN_POINT('',(1.97,-1.7,0.46));
#16436=CARTESIAN_POINT('',(3.07,-1.7,0.46));
#16437=CARTESIAN_POINT('',(3.07,-1.7,0.46));
#16438=CARTESIAN_POINT('',(1.97,-1.7,0.46));
#16439=CARTESIAN_POINT('Origin',(1.97,-1.7,2.3));
#16440=CARTESIAN_POINT('',(1.97,-1.7,2.3));
#16441=CARTESIAN_POINT('',(3.07,-1.7,2.3));
#16442=CARTESIAN_POINT('Origin',(3.07,0.,1.38));
#16443=CARTESIAN_POINT('Origin',(1.97,0.,1.38));
#16444=CARTESIAN_POINT('',(0.,0.,0.));
#16445=CARTESIAN_POINT('Origin',(-1.97,-0.78,0.46));
#16446=CARTESIAN_POINT('',(-1.97,-1.7,0.46));
#16447=CARTESIAN_POINT('',(-1.97,-0.78,0.46));
#16448=CARTESIAN_POINT('',(-1.97,-1.7,0.46));
#16449=CARTESIAN_POINT('',(-3.07,-1.7,0.46));
#16450=CARTESIAN_POINT('',(-1.97,-1.7,0.46));
#16451=CARTESIAN_POINT('',(-3.07,-0.78,0.46));
#16452=CARTESIAN_POINT('',(-3.07,-1.7,0.46));
#16453=CARTESIAN_POINT('',(-1.97,-0.78,0.46));
#16454=CARTESIAN_POINT('Origin',(-1.97,-0.78,1.55));
#16455=CARTESIAN_POINT('',(-1.97,-0.78,1.55));
#16456=CARTESIAN_POINT('',(-1.97,-0.78,0.46));
#16457=CARTESIAN_POINT('',(-3.07,-0.78,1.55));
#16458=CARTESIAN_POINT('',(-3.07,-0.78,0.46));
#16459=CARTESIAN_POINT('',(-1.97,-0.78,1.55));
#16460=CARTESIAN_POINT('Origin',(-1.97,0.78,1.55));
#16461=CARTESIAN_POINT('',(-1.97,0.78,1.55));
#16462=CARTESIAN_POINT('',(-1.97,-0.78,1.55));
#16463=CARTESIAN_POINT('',(-3.07,0.78,1.55));
#16464=CARTESIAN_POINT('',(-3.07,-0.78,1.55));
#16465=CARTESIAN_POINT('',(-1.97,0.78,1.55));
#16466=CARTESIAN_POINT('Origin',(-1.97,0.78,0.46));
#16467=CARTESIAN_POINT('',(-1.97,0.78,0.46));
#16468=CARTESIAN_POINT('',(-1.97,0.78,1.55));
#16469=CARTESIAN_POINT('',(-3.07,0.78,0.46));
#16470=CARTESIAN_POINT('',(-3.07,0.78,1.55));
#16471=CARTESIAN_POINT('',(-1.97,0.78,0.46));
#16472=CARTESIAN_POINT('Origin',(-1.97,1.7,0.46));
#16473=CARTESIAN_POINT('',(-1.97,1.7,0.46));
#16474=CARTESIAN_POINT('',(-1.97,0.78,0.46));
#16475=CARTESIAN_POINT('',(-3.07,1.7,0.46));
#16476=CARTESIAN_POINT('',(-3.07,0.78,0.46));
#16477=CARTESIAN_POINT('',(-1.97,1.7,0.46));
#16478=CARTESIAN_POINT('Origin',(-1.97,1.7,2.3));
#16479=CARTESIAN_POINT('',(-1.97,1.7,2.3));
#16480=CARTESIAN_POINT('',(-1.97,1.7,0.46));
#16481=CARTESIAN_POINT('',(-3.07,1.7,2.3));
#16482=CARTESIAN_POINT('',(-3.07,1.7,0.46));
#16483=CARTESIAN_POINT('',(-1.97,1.7,2.3));
#16484=CARTESIAN_POINT('Origin',(-1.97,-1.7,2.3));
#16485=CARTESIAN_POINT('',(-1.97,-1.7,2.3));
#16486=CARTESIAN_POINT('',(-1.97,1.7,2.3));
#16487=CARTESIAN_POINT('',(-3.07,-1.7,2.3));
#16488=CARTESIAN_POINT('',(-3.07,1.7,2.3));
#16489=CARTESIAN_POINT('',(-1.97,-1.7,2.3));
#16490=CARTESIAN_POINT('Origin',(-1.97,-1.7,0.46));
#16491=CARTESIAN_POINT('',(-1.97,-1.7,2.3));
#16492=CARTESIAN_POINT('',(-3.07,-1.7,2.3));
#16493=CARTESIAN_POINT('Origin',(-1.97,0.,1.38));
#16494=CARTESIAN_POINT('Origin',(-3.07,0.,1.38));
#16495=CARTESIAN_POINT('',(0.,0.,0.));
#16496=CARTESIAN_POINT('',(0.,0.,0.));
#16497=CARTESIAN_POINT('',(0.,0.,0.));
#16498=CARTESIAN_POINT('',(0.,0.,0.));
#16499=CARTESIAN_POINT('Origin',(0.115470053837925,-0.5,-0.2));
#16500=CARTESIAN_POINT('',(0.23094010767585,-0.5,0.));
#16501=CARTESIAN_POINT('',(0.115470053837925,-0.5,-0.2));
#16502=CARTESIAN_POINT('',(0.23094010767585,-0.5,0.));
#16503=CARTESIAN_POINT('',(0.115470053837925,-0.8,-0.2));
#16504=CARTESIAN_POINT('',(0.115470053837925,-0.5,-0.2));
#16505=CARTESIAN_POINT('',(0.23094010767585,-0.8,0.));
#16506=CARTESIAN_POINT('',(0.23094010767585,-0.8,0.));
#16507=CARTESIAN_POINT('',(0.23094010767585,-0.5,0.));
#16508=CARTESIAN_POINT('Origin',(-0.115470053837925,-0.5,-0.2));
#16509=CARTESIAN_POINT('',(-0.115470053837925,-0.5,-0.2));
#16510=CARTESIAN_POINT('',(0.115470053837925,-0.5,-0.2));
#16511=CARTESIAN_POINT('',(-0.115470053837925,-0.8,-0.2));
#16512=CARTESIAN_POINT('',(-0.115470053837925,-0.5,-0.2));
#16513=CARTESIAN_POINT('',(0.115470053837925,-0.8,-0.2));
#16514=CARTESIAN_POINT('Origin',(-0.23094010767585,-0.5,-2.77555756156289E-17));
#16515=CARTESIAN_POINT('',(-0.23094010767585,-0.5,-2.82820063659975E-17));
#16516=CARTESIAN_POINT('',(-0.115470053837925,-0.5,-0.2));
#16517=CARTESIAN_POINT('',(-0.23094010767585,-0.8,-2.77555756156289E-17));
#16518=CARTESIAN_POINT('',(-0.23094010767585,-0.5,-2.82820063659975E-17));
#16519=CARTESIAN_POINT('',(-0.115470053837925,-0.8,-0.2));
#16520=CARTESIAN_POINT('Origin',(-0.115470053837925,-0.5,0.2));
#16521=CARTESIAN_POINT('',(-0.115470053837925,-0.5,0.2));
#16522=CARTESIAN_POINT('',(-0.23094010767585,-0.5,-2.82820063659975E-17));
#16523=CARTESIAN_POINT('',(-0.115470053837925,-0.8,0.2));
#16524=CARTESIAN_POINT('',(-0.115470053837925,-0.5,0.2));
#16525=CARTESIAN_POINT('',(-0.23094010767585,-0.8,-2.82820063659975E-17));
#16526=CARTESIAN_POINT('Origin',(0.115470053837925,-0.5,0.2));
#16527=CARTESIAN_POINT('',(0.115470053837925,-0.5,0.2));
#16528=CARTESIAN_POINT('',(-0.115470053837925,-0.5,0.2));
#16529=CARTESIAN_POINT('',(0.115470053837925,-0.8,0.2));
#16530=CARTESIAN_POINT('',(0.115470053837925,-0.5,0.2));
#16531=CARTESIAN_POINT('',(-0.115470053837925,-0.8,0.2));
#16532=CARTESIAN_POINT('Origin',(0.23094010767585,-0.5,0.));
#16533=CARTESIAN_POINT('',(0.115470053837925,-0.5,0.2));
#16534=CARTESIAN_POINT('',(0.115470053837925,-0.8,0.2));
#16535=CARTESIAN_POINT('Origin',(0.,-0.5,0.));
#16536=CARTESIAN_POINT('Origin',(0.,-0.8,0.));
#16537=CARTESIAN_POINT('Origin',(0.,-1.4,0.));
#16538=CARTESIAN_POINT('',(-0.24505,-1.4,3.00099698131059E-17));
#16539=CARTESIAN_POINT('Origin',(0.,-1.4,0.));
#16540=CARTESIAN_POINT('Origin',(0.375,0.5,0.));
#16541=CARTESIAN_POINT('',(-0.375,0.5,-4.59242549680257E-17));
#16542=CARTESIAN_POINT('Origin',(0.,0.5,0.));
#16543=CARTESIAN_POINT('Origin',(0.,0.475,0.));
#16544=CARTESIAN_POINT('',(-0.425,0.45,-5.20474889637625E-17));
#16545=CARTESIAN_POINT('Origin',(0.,0.45,0.));
#16546=CARTESIAN_POINT('',(-0.4,0.475,-4.89858719658941E-17));
#16547=CARTESIAN_POINT('Origin',(0.,0.24,0.));
#16548=CARTESIAN_POINT('',(-0.425,0.0299999999999998,-5.20474889637625E-17));
#16549=CARTESIAN_POINT('Origin',(0.,0.0299999999999998,0.));
#16550=CARTESIAN_POINT('',(-0.425,0.24,-5.20474889637625E-17));
#16551=CARTESIAN_POINT('Origin',(0.,0.0150000000000001,0.));
#16552=CARTESIAN_POINT('',(-0.395,4.85722573273506E-17,-4.83735485663204E-17));
#16553=CARTESIAN_POINT('Origin',(0.,0.,0.));
#16554=CARTESIAN_POINT('',(-0.41,0.0150000000000001,-5.02105187650415E-17));
#16555=CARTESIAN_POINT('Origin',(0.27,0.,0.));
#16556=CARTESIAN_POINT('',(-0.27,0.,-3.30654635769785E-17));
#16557=CARTESIAN_POINT('Origin',(0.,0.,0.));
#16558=CARTESIAN_POINT('Origin',(0.,-0.02,0.));
#16559=CARTESIAN_POINT('',(-0.24505,-0.0498999999999999,3.00099698131059E-17));
#16560=CARTESIAN_POINT('Origin',(0.,-0.0498999999999999,0.));
#16561=CARTESIAN_POINT('',(-0.26,-0.02,-3.18408167778312E-17));
#16562=CARTESIAN_POINT('Origin',(0.,-0.995,0.));
#16563=CARTESIAN_POINT('',(-0.24505,-0.995,-3.00099698131059E-17));
#16564=CARTESIAN_POINT('',(0.,0.,0.));
#16565=CARTESIAN_POINT('Origin',(0.,0.09,0.));
#16566=CARTESIAN_POINT('',(-0.285,0.1,3.49024337756996E-17));
#16567=CARTESIAN_POINT('Origin',(0.,0.1,0.));
#16568=CARTESIAN_POINT('',(-0.265,0.08,-3.24531401774049E-17));
#16569=CARTESIAN_POINT('',(-0.275,0.09,3.36777869765522E-17));
#16570=CARTESIAN_POINT('Origin',(0.,0.08,0.));
#16571=CARTESIAN_POINT('Origin',(0.,0.,0.));
#16572=CARTESIAN_POINT('',(-0.265,0.,3.24531401774049E-17));
#16573=CARTESIAN_POINT('',(-0.265,0.,3.24531401774049E-17));
#16574=CARTESIAN_POINT('Origin',(0.,0.,0.));
#16575=CARTESIAN_POINT('Origin',(0.,0.1,0.));
#16576=CARTESIAN_POINT('',(-0.5,0.1,6.12323399573677E-17));
#16577=CARTESIAN_POINT('Origin',(0.,0.1,0.));
#16578=CARTESIAN_POINT('Origin',(0.,0.,0.));
#16579=CARTESIAN_POINT('',(-0.5,0.,6.12323399573677E-17));
#16580=CARTESIAN_POINT('',(-0.5,0.,6.12323399573677E-17));
#16581=CARTESIAN_POINT('Origin',(0.,0.,0.));
#16582=CARTESIAN_POINT('Origin',(0.,0.,0.));
#16583=CARTESIAN_POINT('',(0.,0.,0.));
#16584=CARTESIAN_POINT('Origin',(0.375,0.5,0.));
#16585=CARTESIAN_POINT('',(-0.375,0.5,-4.59242549680257E-17));
#16586=CARTESIAN_POINT('Origin',(0.,0.5,0.));
#16587=CARTESIAN_POINT('Origin',(0.,0.475,0.));
#16588=CARTESIAN_POINT('',(-0.425,0.45,-5.20474889637625E-17));
#16589=CARTESIAN_POINT('Origin',(0.,0.45,0.));
#16590=CARTESIAN_POINT('',(-0.4,0.475,-4.89858719658941E-17));
#16591=CARTESIAN_POINT('Origin',(0.,0.24,0.));
#16592=CARTESIAN_POINT('',(-0.425,0.0299999999999998,-5.20474889637625E-17));
#16593=CARTESIAN_POINT('Origin',(0.,0.0299999999999998,0.));
#16594=CARTESIAN_POINT('',(-0.425,0.24,-5.20474889637625E-17));
#16595=CARTESIAN_POINT('Origin',(0.,0.0150000000000001,0.));
#16596=CARTESIAN_POINT('',(-0.395,4.85722573273506E-17,-4.83735485663204E-17));
#16597=CARTESIAN_POINT('Origin',(0.,0.,0.));
#16598=CARTESIAN_POINT('',(-0.41,0.0150000000000001,-5.02105187650415E-17));
#16599=CARTESIAN_POINT('Origin',(0.27,0.,0.));
#16600=CARTESIAN_POINT('',(-0.27,0.,-3.30654635769785E-17));
#16601=CARTESIAN_POINT('Origin',(0.,0.,0.));
#16602=CARTESIAN_POINT('Origin',(0.,-0.02,0.));
#16603=CARTESIAN_POINT('',(-0.24505,-0.0498999999999999,3.00099698131059E-17));
#16604=CARTESIAN_POINT('Origin',(0.,-0.0498999999999999,0.));
#16605=CARTESIAN_POINT('',(-0.26,-0.02,-3.18408167778312E-17));
#16606=CARTESIAN_POINT('Origin',(0.,-0.995,0.));
#16607=CARTESIAN_POINT('',(-0.24505,-1.95495,3.00099698131059E-17));
#16608=CARTESIAN_POINT('Origin',(0.,-1.95495,0.));
#16609=CARTESIAN_POINT('',(-0.24505,-0.995,-3.00099698131059E-17));
#16610=CARTESIAN_POINT('Origin',(0.,-1.975,0.));
#16611=CARTESIAN_POINT('',(-0.2,-2.,-2.44929359829471E-17));
#16612=CARTESIAN_POINT('Origin',(0.,-2.,0.));
#16613=CARTESIAN_POINT('',(-0.225,-1.975,-2.75545529808154E-17));
#16614=CARTESIAN_POINT('Origin',(0.,-2.,0.));
#16615=CARTESIAN_POINT('Origin',(0.115470053837925,-0.5,-0.2));
#16616=CARTESIAN_POINT('',(0.23094010767585,-0.5,0.));
#16617=CARTESIAN_POINT('',(0.115470053837925,-0.5,-0.2));
#16618=CARTESIAN_POINT('',(0.23094010767585,-0.5,0.));
#16619=CARTESIAN_POINT('',(0.115470053837925,-0.8,-0.2));
#16620=CARTESIAN_POINT('',(0.115470053837925,-0.5,-0.2));
#16621=CARTESIAN_POINT('',(0.23094010767585,-0.8,0.));
#16622=CARTESIAN_POINT('',(0.23094010767585,-0.8,0.));
#16623=CARTESIAN_POINT('',(0.23094010767585,-0.5,0.));
#16624=CARTESIAN_POINT('Origin',(-0.115470053837925,-0.5,-0.2));
#16625=CARTESIAN_POINT('',(-0.115470053837925,-0.5,-0.2));
#16626=CARTESIAN_POINT('',(0.115470053837925,-0.5,-0.2));
#16627=CARTESIAN_POINT('',(-0.115470053837925,-0.8,-0.2));
#16628=CARTESIAN_POINT('',(-0.115470053837925,-0.5,-0.2));
#16629=CARTESIAN_POINT('',(0.115470053837925,-0.8,-0.2));
#16630=CARTESIAN_POINT('Origin',(-0.23094010767585,-0.5,-2.77555756156289E-17));
#16631=CARTESIAN_POINT('',(-0.23094010767585,-0.5,-2.82820063659975E-17));
#16632=CARTESIAN_POINT('',(-0.115470053837925,-0.5,-0.2));
#16633=CARTESIAN_POINT('',(-0.23094010767585,-0.8,-2.77555756156289E-17));
#16634=CARTESIAN_POINT('',(-0.23094010767585,-0.5,-2.82820063659975E-17));
#16635=CARTESIAN_POINT('',(-0.115470053837925,-0.8,-0.2));
#16636=CARTESIAN_POINT('Origin',(-0.115470053837925,-0.5,0.2));
#16637=CARTESIAN_POINT('',(-0.115470053837925,-0.5,0.2));
#16638=CARTESIAN_POINT('',(-0.23094010767585,-0.5,-2.82820063659975E-17));
#16639=CARTESIAN_POINT('',(-0.115470053837925,-0.8,0.2));
#16640=CARTESIAN_POINT('',(-0.115470053837925,-0.5,0.2));
#16641=CARTESIAN_POINT('',(-0.23094010767585,-0.8,-2.82820063659975E-17));
#16642=CARTESIAN_POINT('Origin',(0.115470053837925,-0.5,0.2));
#16643=CARTESIAN_POINT('',(0.115470053837925,-0.5,0.2));
#16644=CARTESIAN_POINT('',(-0.115470053837925,-0.5,0.2));
#16645=CARTESIAN_POINT('',(0.115470053837925,-0.8,0.2));
#16646=CARTESIAN_POINT('',(0.115470053837925,-0.5,0.2));
#16647=CARTESIAN_POINT('',(-0.115470053837925,-0.8,0.2));
#16648=CARTESIAN_POINT('Origin',(0.23094010767585,-0.5,0.));
#16649=CARTESIAN_POINT('',(0.115470053837925,-0.5,0.2));
#16650=CARTESIAN_POINT('',(0.115470053837925,-0.8,0.2));
#16651=CARTESIAN_POINT('Origin',(0.,-0.5,0.));
#16652=CARTESIAN_POINT('Origin',(0.,-0.8,0.));
#16653=CARTESIAN_POINT('',(0.,0.,0.));
#16654=CARTESIAN_POINT('',(0.,0.,0.));
#16655=CARTESIAN_POINT('',(0.,0.,0.));
#16656=CARTESIAN_POINT('',(0.,0.,0.));
#16657=CARTESIAN_POINT('',(0.,0.,0.));
#16658=CARTESIAN_POINT('',(0.,0.,0.));
#16659=CARTESIAN_POINT('',(0.,0.,0.));
#16660=CARTESIAN_POINT('',(0.,0.,0.));
#16661=CARTESIAN_POINT('',(0.,0.,0.));
#16662=CARTESIAN_POINT('',(0.,0.,0.));
#16663=CARTESIAN_POINT('',(-5.8,-16.5,2.2));
#16664=CARTESIAN_POINT('',(-5.8,-13.5,2.2));
#16665=CARTESIAN_POINT('',(5.8,-16.5,2.2));
#16666=CARTESIAN_POINT('',(5.8,-13.5,2.2));
#16667=CARTESIAN_POINT('',(0.,-15.,12.));
#16668=CARTESIAN_POINT('',(-4.75,-15.,9.87));
#16669=CARTESIAN_POINT('',(-4.75,-15.,10.03));
#16670=CARTESIAN_POINT('',(4.75,-15.,9.87));
#16671=CARTESIAN_POINT('',(4.75,-15.,10.03));
#16672=CARTESIAN_POINT('',(-5.8,-8.5,2.2));
#16673=CARTESIAN_POINT('',(-5.8,-5.5,2.2));
#16674=CARTESIAN_POINT('',(5.8,-8.5,2.2));
#16675=CARTESIAN_POINT('',(5.8,-5.5,2.2));
#16676=CARTESIAN_POINT('',(0.,-7.,12.));
#16677=CARTESIAN_POINT('',(-4.75,-7.,9.87));
#16678=CARTESIAN_POINT('',(-4.75,-7.,10.03));
#16679=CARTESIAN_POINT('',(4.75,-7.,9.87));
#16680=CARTESIAN_POINT('',(4.75,-7.,10.03));
#16681=CARTESIAN_POINT('',(3.,-2.4,2.2));
#16682=CARTESIAN_POINT('',(3.,2.4,2.2));
#16683=CARTESIAN_POINT('',(23.,-2.4,2.2));
#16684=CARTESIAN_POINT('',(23.,2.4,2.2));
#16685=CARTESIAN_POINT('',(2.,0.,4.3));
#16686=CARTESIAN_POINT('',(4.,0.,5.27));
#16687=CARTESIAN_POINT('',(10.,0.,5.27));
#16688=CARTESIAN_POINT('',(16.,0.,5.27));
#16689=CARTESIAN_POINT('',(22.,0.,5.27));
#16690=CARTESIAN_POINT('',(0.,0.,0.));
#16691=CARTESIAN_POINT('Origin',(0.0866025403784439,-0.4,-0.15));
#16692=CARTESIAN_POINT('',(0.173205080756888,-0.4,0.));
#16693=CARTESIAN_POINT('',(0.0866025403784439,-0.4,-0.15));
#16694=CARTESIAN_POINT('',(0.173205080756888,-0.4,0.));
#16695=CARTESIAN_POINT('',(0.0866025403784439,-0.64,-0.15));
#16696=CARTESIAN_POINT('',(0.0866025403784439,-0.4,-0.15));
#16697=CARTESIAN_POINT('',(0.173205080756888,-0.64,0.));
#16698=CARTESIAN_POINT('',(0.173205080756888,-0.64,0.));
#16699=CARTESIAN_POINT('',(0.173205080756888,-0.4,0.));
#16700=CARTESIAN_POINT('Origin',(-0.0866025403784438,-0.4,-0.15));
#16701=CARTESIAN_POINT('',(-0.0866025403784438,-0.4,-0.15));
#16702=CARTESIAN_POINT('',(0.0866025403784439,-0.4,-0.15));
#16703=CARTESIAN_POINT('',(-0.0866025403784438,-0.64,-0.15));
#16704=CARTESIAN_POINT('',(-0.0866025403784438,-0.4,-0.15));
#16705=CARTESIAN_POINT('',(0.0866025403784439,-0.64,-0.15));
#16706=CARTESIAN_POINT('Origin',(-0.173205080756888,-0.4,-2.77555756156289E-17));
#16707=CARTESIAN_POINT('',(-0.173205080756888,-0.4,-2.12115047744981E-17));
#16708=CARTESIAN_POINT('',(-0.0866025403784438,-0.4,-0.15));
#16709=CARTESIAN_POINT('',(-0.173205080756888,-0.64,-2.77555756156289E-17));
#16710=CARTESIAN_POINT('',(-0.173205080756888,-0.4,-2.12115047744981E-17));
#16711=CARTESIAN_POINT('',(-0.0866025403784438,-0.64,-0.15));
#16712=CARTESIAN_POINT('Origin',(-0.0866025403784439,-0.4,0.15));
#16713=CARTESIAN_POINT('',(-0.0866025403784439,-0.4,0.15));
#16714=CARTESIAN_POINT('',(-0.173205080756888,-0.4,-2.12115047744981E-17));
#16715=CARTESIAN_POINT('',(-0.0866025403784439,-0.64,0.15));
#16716=CARTESIAN_POINT('',(-0.0866025403784439,-0.4,0.15));
#16717=CARTESIAN_POINT('',(-0.173205080756888,-0.64,-2.12115047744981E-17));
#16718=CARTESIAN_POINT('Origin',(0.0866025403784439,-0.4,0.15));
#16719=CARTESIAN_POINT('',(0.0866025403784439,-0.4,0.15));
#16720=CARTESIAN_POINT('',(-0.0866025403784439,-0.4,0.15));
#16721=CARTESIAN_POINT('',(0.0866025403784439,-0.64,0.15));
#16722=CARTESIAN_POINT('',(0.0866025403784439,-0.4,0.15));
#16723=CARTESIAN_POINT('',(-0.0866025403784439,-0.64,0.15));
#16724=CARTESIAN_POINT('Origin',(0.173205080756888,-0.4,0.));
#16725=CARTESIAN_POINT('',(0.0866025403784439,-0.4,0.15));
#16726=CARTESIAN_POINT('',(0.0866025403784439,-0.64,0.15));
#16727=CARTESIAN_POINT('Origin',(0.,-0.4,-2.77555756156289E-17));
#16728=CARTESIAN_POINT('Origin',(0.,-0.64,-2.77555756156289E-17));
#16729=CARTESIAN_POINT('Origin',(0.,-1.,0.));
#16730=CARTESIAN_POINT('',(-0.1954,-1.,2.39295984553393E-17));
#16731=CARTESIAN_POINT('Origin',(0.,-1.,0.));
#16732=CARTESIAN_POINT('Origin',(0.3,0.4,0.));
#16733=CARTESIAN_POINT('',(-0.3,0.4,-3.67394039744206E-17));
#16734=CARTESIAN_POINT('Origin',(0.,0.4,0.));
#16735=CARTESIAN_POINT('Origin',(0.,0.375,0.));
#16736=CARTESIAN_POINT('',(-0.35,0.35,-4.28626379701573E-17));
#16737=CARTESIAN_POINT('Origin',(0.,0.35,0.));
#16738=CARTESIAN_POINT('',(-0.325,0.375,-3.9801020972289E-17));
#16739=CARTESIAN_POINT('Origin',(0.,0.19,0.));
#16740=CARTESIAN_POINT('',(-0.35,0.03,-4.28626379701574E-17));
#16741=CARTESIAN_POINT('Origin',(0.,0.03,0.));
#16742=CARTESIAN_POINT('',(-0.35,0.19,-4.28626379701574E-17));
#16743=CARTESIAN_POINT('Origin',(0.,0.0149999999999999,0.));
#16744=CARTESIAN_POINT('',(-0.32,-3.29597460435593E-17,-3.91886975727153E-17));
#16745=CARTESIAN_POINT('Origin',(0.,0.,0.));
#16746=CARTESIAN_POINT('',(-0.335,0.0149999999999999,-4.10256677714363E-17));
#16747=CARTESIAN_POINT('Origin',(0.22,0.,0.));
#16748=CARTESIAN_POINT('',(-0.22,-6.93889390390723E-18,-2.69422295812418E-17));
#16749=CARTESIAN_POINT('Origin',(0.,0.,0.));
#16750=CARTESIAN_POINT('Origin',(0.,-0.02,0.));
#16751=CARTESIAN_POINT('',(-0.1954,-0.0492,2.39295984553393E-17));
#16752=CARTESIAN_POINT('Origin',(0.,-0.0492,0.));
#16753=CARTESIAN_POINT('',(-0.21,-0.02,-2.57175827820944E-17));
#16754=CARTESIAN_POINT('Origin',(0.,-0.8,0.));
#16755=CARTESIAN_POINT('',(-0.1954,-0.8,-2.39295984553393E-17));
#16756=CARTESIAN_POINT('',(0.,0.,0.));
#16757=CARTESIAN_POINT('',(0.,0.,0.));
#16758=CARTESIAN_POINT('',(0.,0.,0.));
#16759=CARTESIAN_POINT('',(0.,0.,0.));
#16760=CARTESIAN_POINT('',(0.,0.,0.));
#16761=CARTESIAN_POINT('',(0.,0.,0.));
#16762=CARTESIAN_POINT('',(0.,0.,0.));
#16763=CARTESIAN_POINT('',(0.,0.,0.));
#16764=CARTESIAN_POINT('',(0.,0.,0.));
#16765=CARTESIAN_POINT('',(0.,-0.5,11.35));
#16766=CARTESIAN_POINT('',(0.,-17.05,13.8));
#16767=CARTESIAN_POINT('',(0.,-4.15,13.8));
#16768=CARTESIAN_POINT('',(0.,-1.3,13.8));
#16769=CARTESIAN_POINT('',(1.,5.,12.));
#16770=CARTESIAN_POINT('',(0.,0.,0.));
#16771=CARTESIAN_POINT('',(0.,0.,0.));
#16772=CARTESIAN_POINT('',(0.,0.,0.));
#16773=CARTESIAN_POINT('',(0.,0.,0.));
#16774=CARTESIAN_POINT('',(0.,0.,0.));
#16775=CARTESIAN_POINT('',(0.,0.,0.));
#16776=CARTESIAN_POINT('',(11.,0.,4.3));
#16777=CARTESIAN_POINT('',(9.5,-1.9,7.5));
#16778=CARTESIAN_POINT('',(9.5,-1.9,7.6));
#16779=CARTESIAN_POINT('',(9.5,1.9,7.5));
#16780=CARTESIAN_POINT('',(9.5,1.9,7.6));
#16781=CARTESIAN_POINT('',(12.5,-1.9,7.5));
#16782=CARTESIAN_POINT('',(12.5,-1.9,7.6));
#16783=CARTESIAN_POINT('',(12.5,1.9,7.5));
#16784=CARTESIAN_POINT('',(12.5,1.9,7.6));
#16785=CARTESIAN_POINT('',(11.,-3.2,9.5));
#16786=CARTESIAN_POINT('',(11.,-3.2,9.6));
#16787=CARTESIAN_POINT('',(11.,0.2,9.5));
#16788=CARTESIAN_POINT('',(11.,0.199999999999999,9.6));
#16789=CARTESIAN_POINT('',(11.,5.,12.));
#16790=CARTESIAN_POINT('',(0.,0.,0.));
#16791=CARTESIAN_POINT('',(0.,0.,0.));
#16792=CARTESIAN_POINT('',(0.,0.,0.));
#16793=CARTESIAN_POINT('',(0.,0.,0.));
#16794=UNCERTAINTY_MEASURE_WITH_UNIT(LENGTH_MEASURE(0.001),#16912,
'DISTANCE_ACCURACY_VALUE',
'Maximum model space distance between geometric entities at asserted c
onnectivities');
#16795=UNCERTAINTY_MEASURE_WITH_UNIT(LENGTH_MEASURE(0.001),#16912,
'DISTANCE_ACCURACY_VALUE',
'Maximum model space distance between geometric entities at asserted c
onnectivities');
#16796=UNCERTAINTY_MEASURE_WITH_UNIT(LENGTH_MEASURE(0.001),#16912,
'DISTANCE_ACCURACY_VALUE',
'Maximum model space distance between geometric entities at asserted c
onnectivities');
#16797=UNCERTAINTY_MEASURE_WITH_UNIT(LENGTH_MEASURE(0.001),#16912,
'DISTANCE_ACCURACY_VALUE',
'Maximum model space distance between geometric entities at asserted c
onnectivities');
#16798=UNCERTAINTY_MEASURE_WITH_UNIT(LENGTH_MEASURE(0.001),#16912,
'DISTANCE_ACCURACY_VALUE',
'Maximum model space distance between geometric entities at asserted c
onnectivities');
#16799=UNCERTAINTY_MEASURE_WITH_UNIT(LENGTH_MEASURE(0.001),#16912,
'DISTANCE_ACCURACY_VALUE',
'Maximum model space distance between geometric entities at asserted c
onnectivities');
#16800=UNCERTAINTY_MEASURE_WITH_UNIT(LENGTH_MEASURE(0.001),#16912,
'DISTANCE_ACCURACY_VALUE',
'Maximum model space distance between geometric entities at asserted c
onnectivities');
#16801=UNCERTAINTY_MEASURE_WITH_UNIT(LENGTH_MEASURE(0.001),#16912,
'DISTANCE_ACCURACY_VALUE',
'Maximum model space distance between geometric entities at asserted c
onnectivities');
#16802=UNCERTAINTY_MEASURE_WITH_UNIT(LENGTH_MEASURE(0.001),#16912,
'DISTANCE_ACCURACY_VALUE',
'Maximum model space distance between geometric entities at asserted c
onnectivities');
#16803=UNCERTAINTY_MEASURE_WITH_UNIT(LENGTH_MEASURE(0.001),#16912,
'DISTANCE_ACCURACY_VALUE',
'Maximum model space distance between geometric entities at asserted c
onnectivities');
#16804=UNCERTAINTY_MEASURE_WITH_UNIT(LENGTH_MEASURE(0.001),#16912,
'DISTANCE_ACCURACY_VALUE',
'Maximum model space distance between geometric entities at asserted c
onnectivities');
#16805=UNCERTAINTY_MEASURE_WITH_UNIT(LENGTH_MEASURE(0.001),#16912,
'DISTANCE_ACCURACY_VALUE',
'Maximum model space distance between geometric entities at asserted c
onnectivities');
#16806=UNCERTAINTY_MEASURE_WITH_UNIT(LENGTH_MEASURE(0.001),#16912,
'DISTANCE_ACCURACY_VALUE',
'Maximum model space distance between geometric entities at asserted c
onnectivities');
#16807=UNCERTAINTY_MEASURE_WITH_UNIT(LENGTH_MEASURE(0.001),#16912,
'DISTANCE_ACCURACY_VALUE',
'Maximum model space distance between geometric entities at asserted c
onnectivities');
#16808=UNCERTAINTY_MEASURE_WITH_UNIT(LENGTH_MEASURE(0.001),#16912,
'DISTANCE_ACCURACY_VALUE',
'Maximum model space distance between geometric entities at asserted c
onnectivities');
#16809=UNCERTAINTY_MEASURE_WITH_UNIT(LENGTH_MEASURE(0.001),#16912,
'DISTANCE_ACCURACY_VALUE',
'Maximum model space distance between geometric entities at asserted c
onnectivities');
#16810=UNCERTAINTY_MEASURE_WITH_UNIT(LENGTH_MEASURE(0.001),#16912,
'DISTANCE_ACCURACY_VALUE',
'Maximum model space distance between geometric entities at asserted c
onnectivities');
#16811=UNCERTAINTY_MEASURE_WITH_UNIT(LENGTH_MEASURE(0.001),#16912,
'DISTANCE_ACCURACY_VALUE',
'Maximum model space distance between geometric entities at asserted c
onnectivities');
#16812=UNCERTAINTY_MEASURE_WITH_UNIT(LENGTH_MEASURE(0.001),#16912,
'DISTANCE_ACCURACY_VALUE',
'Maximum model space distance between geometric entities at asserted c
onnectivities');
#16813=UNCERTAINTY_MEASURE_WITH_UNIT(LENGTH_MEASURE(0.001),#16912,
'DISTANCE_ACCURACY_VALUE',
'Maximum model space distance between geometric entities at asserted c
onnectivities');
#16814=UNCERTAINTY_MEASURE_WITH_UNIT(LENGTH_MEASURE(0.001),#16912,
'DISTANCE_ACCURACY_VALUE',
'Maximum model space distance between geometric entities at asserted c
onnectivities');
#16815=UNCERTAINTY_MEASURE_WITH_UNIT(LENGTH_MEASURE(0.001),#16912,
'DISTANCE_ACCURACY_VALUE',
'Maximum model space distance between geometric entities at asserted c
onnectivities');
#16816=UNCERTAINTY_MEASURE_WITH_UNIT(LENGTH_MEASURE(0.001),#16912,
'DISTANCE_ACCURACY_VALUE',
'Maximum model space distance between geometric entities at asserted c
onnectivities');
#16817=UNCERTAINTY_MEASURE_WITH_UNIT(LENGTH_MEASURE(0.001),#16912,
'DISTANCE_ACCURACY_VALUE',
'Maximum model space distance between geometric entities at asserted c
onnectivities');
#16818=UNCERTAINTY_MEASURE_WITH_UNIT(LENGTH_MEASURE(0.001),#16912,
'DISTANCE_ACCURACY_VALUE',
'Maximum model space distance between geometric entities at asserted c
onnectivities');
#16819=UNCERTAINTY_MEASURE_WITH_UNIT(LENGTH_MEASURE(0.001),#16912,
'DISTANCE_ACCURACY_VALUE',
'Maximum model space distance between geometric entities at asserted c
onnectivities');
#16820=UNCERTAINTY_MEASURE_WITH_UNIT(LENGTH_MEASURE(0.001),#16912,
'DISTANCE_ACCURACY_VALUE',
'Maximum model space distance between geometric entities at asserted c
onnectivities');
#16821=UNCERTAINTY_MEASURE_WITH_UNIT(LENGTH_MEASURE(0.001),#16912,
'DISTANCE_ACCURACY_VALUE',
'Maximum model space distance between geometric entities at asserted c
onnectivities');
#16822=UNCERTAINTY_MEASURE_WITH_UNIT(LENGTH_MEASURE(0.001),#16912,
'DISTANCE_ACCURACY_VALUE',
'Maximum model space distance between geometric entities at asserted c
onnectivities');
#16823=UNCERTAINTY_MEASURE_WITH_UNIT(LENGTH_MEASURE(0.001),#16912,
'DISTANCE_ACCURACY_VALUE',
'Maximum model space distance between geometric entities at asserted c
onnectivities');
#16824=UNCERTAINTY_MEASURE_WITH_UNIT(LENGTH_MEASURE(0.001),#16912,
'DISTANCE_ACCURACY_VALUE',
'Maximum model space distance between geometric entities at asserted c
onnectivities');
#16825=UNCERTAINTY_MEASURE_WITH_UNIT(LENGTH_MEASURE(0.001),#16912,
'DISTANCE_ACCURACY_VALUE',
'Maximum model space distance between geometric entities at asserted c
onnectivities');
#16826=UNCERTAINTY_MEASURE_WITH_UNIT(LENGTH_MEASURE(0.001),#16912,
'DISTANCE_ACCURACY_VALUE',
'Maximum model space distance between geometric entities at asserted c
onnectivities');
#16827=UNCERTAINTY_MEASURE_WITH_UNIT(LENGTH_MEASURE(0.001),#16912,
'DISTANCE_ACCURACY_VALUE',
'Maximum model space distance between geometric entities at asserted c
onnectivities');
#16828=UNCERTAINTY_MEASURE_WITH_UNIT(LENGTH_MEASURE(0.001),#16912,
'DISTANCE_ACCURACY_VALUE',
'Maximum model space distance between geometric entities at asserted c
onnectivities');
#16829=UNCERTAINTY_MEASURE_WITH_UNIT(LENGTH_MEASURE(0.001),#16912,
'DISTANCE_ACCURACY_VALUE',
'Maximum model space distance between geometric entities at asserted c
onnectivities');
#16830=UNCERTAINTY_MEASURE_WITH_UNIT(LENGTH_MEASURE(0.001),#16912,
'DISTANCE_ACCURACY_VALUE',
'Maximum model space distance between geometric entities at asserted c
onnectivities');
#16831=UNCERTAINTY_MEASURE_WITH_UNIT(LENGTH_MEASURE(0.001),#16912,
'DISTANCE_ACCURACY_VALUE',
'Maximum model space distance between geometric entities at asserted c
onnectivities');
#16832=UNCERTAINTY_MEASURE_WITH_UNIT(LENGTH_MEASURE(0.001),#16912,
'DISTANCE_ACCURACY_VALUE',
'Maximum model space distance between geometric entities at asserted c
onnectivities');
#16833=UNCERTAINTY_MEASURE_WITH_UNIT(LENGTH_MEASURE(0.001),#16912,
'DISTANCE_ACCURACY_VALUE',
'Maximum model space distance between geometric entities at asserted c
onnectivities');
#16834=UNCERTAINTY_MEASURE_WITH_UNIT(LENGTH_MEASURE(0.001),#16912,
'DISTANCE_ACCURACY_VALUE',
'Maximum model space distance between geometric entities at asserted c
onnectivities');
#16835=UNCERTAINTY_MEASURE_WITH_UNIT(LENGTH_MEASURE(0.001),#16912,
'DISTANCE_ACCURACY_VALUE',
'Maximum model space distance between geometric entities at asserted c
onnectivities');
#16836=UNCERTAINTY_MEASURE_WITH_UNIT(LENGTH_MEASURE(0.001),#16912,
'DISTANCE_ACCURACY_VALUE',
'Maximum model space distance between geometric entities at asserted c
onnectivities');
#16837=UNCERTAINTY_MEASURE_WITH_UNIT(LENGTH_MEASURE(0.001),#16912,
'DISTANCE_ACCURACY_VALUE',
'Maximum model space distance between geometric entities at asserted c
onnectivities');
#16838=UNCERTAINTY_MEASURE_WITH_UNIT(LENGTH_MEASURE(0.001),#16912,
'DISTANCE_ACCURACY_VALUE',
'Maximum model space distance between geometric entities at asserted c
onnectivities');
#16839=UNCERTAINTY_MEASURE_WITH_UNIT(LENGTH_MEASURE(0.001),#16912,
'DISTANCE_ACCURACY_VALUE',
'Maximum model space distance between geometric entities at asserted c
onnectivities');
#16840=UNCERTAINTY_MEASURE_WITH_UNIT(LENGTH_MEASURE(0.001),#16912,
'DISTANCE_ACCURACY_VALUE',
'Maximum model space distance between geometric entities at asserted c
onnectivities');
#16841=UNCERTAINTY_MEASURE_WITH_UNIT(LENGTH_MEASURE(0.001),#16912,
'DISTANCE_ACCURACY_VALUE',
'Maximum model space distance between geometric entities at asserted c
onnectivities');
#16842=UNCERTAINTY_MEASURE_WITH_UNIT(LENGTH_MEASURE(0.001),#16912,
'DISTANCE_ACCURACY_VALUE',
'Maximum model space distance between geometric entities at asserted c
onnectivities');
#16843=UNCERTAINTY_MEASURE_WITH_UNIT(LENGTH_MEASURE(0.001),#16912,
'DISTANCE_ACCURACY_VALUE',
'Maximum model space distance between geometric entities at asserted c
onnectivities');
#16844=UNCERTAINTY_MEASURE_WITH_UNIT(LENGTH_MEASURE(0.001),#16912,
'DISTANCE_ACCURACY_VALUE',
'Maximum model space distance between geometric entities at asserted c
onnectivities');
#16845=UNCERTAINTY_MEASURE_WITH_UNIT(LENGTH_MEASURE(0.001),#16912,
'DISTANCE_ACCURACY_VALUE',
'Maximum model space distance between geometric entities at asserted c
onnectivities');
#16846=UNCERTAINTY_MEASURE_WITH_UNIT(LENGTH_MEASURE(0.001),#16912,
'DISTANCE_ACCURACY_VALUE',
'Maximum model space distance between geometric entities at asserted c
onnectivities');
#16847=UNCERTAINTY_MEASURE_WITH_UNIT(LENGTH_MEASURE(0.001),#16912,
'DISTANCE_ACCURACY_VALUE',
'Maximum model space distance between geometric entities at asserted c
onnectivities');
#16848=UNCERTAINTY_MEASURE_WITH_UNIT(LENGTH_MEASURE(0.001),#16912,
'DISTANCE_ACCURACY_VALUE',
'Maximum model space distance between geometric entities at asserted c
onnectivities');
#16849=UNCERTAINTY_MEASURE_WITH_UNIT(LENGTH_MEASURE(0.001),#16912,
'DISTANCE_ACCURACY_VALUE',
'Maximum model space distance between geometric entities at asserted c
onnectivities');
#16850=UNCERTAINTY_MEASURE_WITH_UNIT(LENGTH_MEASURE(0.001),#16912,
'DISTANCE_ACCURACY_VALUE',
'Maximum model space distance between geometric entities at asserted c
onnectivities');
#16851=UNCERTAINTY_MEASURE_WITH_UNIT(LENGTH_MEASURE(0.001),#16912,
'DISTANCE_ACCURACY_VALUE',
'Maximum model space distance between geometric entities at asserted c
onnectivities');
#16852=UNCERTAINTY_MEASURE_WITH_UNIT(LENGTH_MEASURE(0.001),#16912,
'DISTANCE_ACCURACY_VALUE',
'Maximum model space distance between geometric entities at asserted c
onnectivities');
#16853=(
GEOMETRIC_REPRESENTATION_CONTEXT(3)
GLOBAL_UNCERTAINTY_ASSIGNED_CONTEXT((#16794))
GLOBAL_UNIT_ASSIGNED_CONTEXT((#16912,#16914,#16915))
REPRESENTATION_CONTEXT('','3D')
);
#16854=(
GEOMETRIC_REPRESENTATION_CONTEXT(3)
GLOBAL_UNCERTAINTY_ASSIGNED_CONTEXT((#16795))
GLOBAL_UNIT_ASSIGNED_CONTEXT((#16912,#16914,#16915))
REPRESENTATION_CONTEXT('','3D')
);
#16855=(
GEOMETRIC_REPRESENTATION_CONTEXT(3)
GLOBAL_UNCERTAINTY_ASSIGNED_CONTEXT((#16796))
GLOBAL_UNIT_ASSIGNED_CONTEXT((#16912,#16914,#16915))
REPRESENTATION_CONTEXT('','3D')
);
#16856=(
GEOMETRIC_REPRESENTATION_CONTEXT(3)
GLOBAL_UNCERTAINTY_ASSIGNED_CONTEXT((#16797))
GLOBAL_UNIT_ASSIGNED_CONTEXT((#16912,#16914,#16915))
REPRESENTATION_CONTEXT('','3D')
);
#16857=(
GEOMETRIC_REPRESENTATION_CONTEXT(3)
GLOBAL_UNCERTAINTY_ASSIGNED_CONTEXT((#16798))
GLOBAL_UNIT_ASSIGNED_CONTEXT((#16912,#16914,#16915))
REPRESENTATION_CONTEXT('','3D')
);
#16858=(
GEOMETRIC_REPRESENTATION_CONTEXT(3)
GLOBAL_UNCERTAINTY_ASSIGNED_CONTEXT((#16799))
GLOBAL_UNIT_ASSIGNED_CONTEXT((#16912,#16914,#16915))
REPRESENTATION_CONTEXT('','3D')
);
#16859=(
GEOMETRIC_REPRESENTATION_CONTEXT(3)
GLOBAL_UNCERTAINTY_ASSIGNED_CONTEXT((#16800))
GLOBAL_UNIT_ASSIGNED_CONTEXT((#16912,#16914,#16915))
REPRESENTATION_CONTEXT('','3D')
);
#16860=(
GEOMETRIC_REPRESENTATION_CONTEXT(3)
GLOBAL_UNCERTAINTY_ASSIGNED_CONTEXT((#16801))
GLOBAL_UNIT_ASSIGNED_CONTEXT((#16912,#16914,#16915))
REPRESENTATION_CONTEXT('','3D')
);
#16861=(
GEOMETRIC_REPRESENTATION_CONTEXT(3)
GLOBAL_UNCERTAINTY_ASSIGNED_CONTEXT((#16802))
GLOBAL_UNIT_ASSIGNED_CONTEXT((#16912,#16914,#16915))
REPRESENTATION_CONTEXT('','3D')
);
#16862=(
GEOMETRIC_REPRESENTATION_CONTEXT(3)
GLOBAL_UNCERTAINTY_ASSIGNED_CONTEXT((#16803))
GLOBAL_UNIT_ASSIGNED_CONTEXT((#16912,#16914,#16915))
REPRESENTATION_CONTEXT('','3D')
);
#16863=(
GEOMETRIC_REPRESENTATION_CONTEXT(3)
GLOBAL_UNCERTAINTY_ASSIGNED_CONTEXT((#16804))
GLOBAL_UNIT_ASSIGNED_CONTEXT((#16912,#16914,#16915))
REPRESENTATION_CONTEXT('','3D')
);
#16864=(
GEOMETRIC_REPRESENTATION_CONTEXT(3)
GLOBAL_UNCERTAINTY_ASSIGNED_CONTEXT((#16805))
GLOBAL_UNIT_ASSIGNED_CONTEXT((#16912,#16914,#16915))
REPRESENTATION_CONTEXT('','3D')
);
#16865=(
GEOMETRIC_REPRESENTATION_CONTEXT(3)
GLOBAL_UNCERTAINTY_ASSIGNED_CONTEXT((#16806))
GLOBAL_UNIT_ASSIGNED_CONTEXT((#16912,#16914,#16915))
REPRESENTATION_CONTEXT('','3D')
);
#16866=(
GEOMETRIC_REPRESENTATION_CONTEXT(3)
GLOBAL_UNCERTAINTY_ASSIGNED_CONTEXT((#16807))
GLOBAL_UNIT_ASSIGNED_CONTEXT((#16912,#16914,#16915))
REPRESENTATION_CONTEXT('','3D')
);
#16867=(
GEOMETRIC_REPRESENTATION_CONTEXT(3)
GLOBAL_UNCERTAINTY_ASSIGNED_CONTEXT((#16808))
GLOBAL_UNIT_ASSIGNED_CONTEXT((#16912,#16914,#16915))
REPRESENTATION_CONTEXT('','3D')
);
#16868=(
GEOMETRIC_REPRESENTATION_CONTEXT(3)
GLOBAL_UNCERTAINTY_ASSIGNED_CONTEXT((#16809))
GLOBAL_UNIT_ASSIGNED_CONTEXT((#16912,#16914,#16915))
REPRESENTATION_CONTEXT('','3D')
);
#16869=(
GEOMETRIC_REPRESENTATION_CONTEXT(3)
GLOBAL_UNCERTAINTY_ASSIGNED_CONTEXT((#16810))
GLOBAL_UNIT_ASSIGNED_CONTEXT((#16912,#16914,#16915))
REPRESENTATION_CONTEXT('','3D')
);
#16870=(
GEOMETRIC_REPRESENTATION_CONTEXT(3)
GLOBAL_UNCERTAINTY_ASSIGNED_CONTEXT((#16811))
GLOBAL_UNIT_ASSIGNED_CONTEXT((#16912,#16914,#16915))
REPRESENTATION_CONTEXT('','3D')
);
#16871=(
GEOMETRIC_REPRESENTATION_CONTEXT(3)
GLOBAL_UNCERTAINTY_ASSIGNED_CONTEXT((#16812))
GLOBAL_UNIT_ASSIGNED_CONTEXT((#16912,#16914,#16915))
REPRESENTATION_CONTEXT('','3D')
);
#16872=(
GEOMETRIC_REPRESENTATION_CONTEXT(3)
GLOBAL_UNCERTAINTY_ASSIGNED_CONTEXT((#16813))
GLOBAL_UNIT_ASSIGNED_CONTEXT((#16912,#16914,#16915))
REPRESENTATION_CONTEXT('','3D')
);
#16873=(
GEOMETRIC_REPRESENTATION_CONTEXT(3)
GLOBAL_UNCERTAINTY_ASSIGNED_CONTEXT((#16814))
GLOBAL_UNIT_ASSIGNED_CONTEXT((#16912,#16914,#16915))
REPRESENTATION_CONTEXT('','3D')
);
#16874=(
GEOMETRIC_REPRESENTATION_CONTEXT(3)
GLOBAL_UNCERTAINTY_ASSIGNED_CONTEXT((#16815))
GLOBAL_UNIT_ASSIGNED_CONTEXT((#16912,#16914,#16915))
REPRESENTATION_CONTEXT('','3D')
);
#16875=(
GEOMETRIC_REPRESENTATION_CONTEXT(3)
GLOBAL_UNCERTAINTY_ASSIGNED_CONTEXT((#16816))
GLOBAL_UNIT_ASSIGNED_CONTEXT((#16912,#16914,#16915))
REPRESENTATION_CONTEXT('','3D')
);
#16876=(
GEOMETRIC_REPRESENTATION_CONTEXT(3)
GLOBAL_UNCERTAINTY_ASSIGNED_CONTEXT((#16817))
GLOBAL_UNIT_ASSIGNED_CONTEXT((#16912,#16914,#16915))
REPRESENTATION_CONTEXT('','3D')
);
#16877=(
GEOMETRIC_REPRESENTATION_CONTEXT(3)
GLOBAL_UNCERTAINTY_ASSIGNED_CONTEXT((#16818))
GLOBAL_UNIT_ASSIGNED_CONTEXT((#16912,#16914,#16915))
REPRESENTATION_CONTEXT('','3D')
);
#16878=(
GEOMETRIC_REPRESENTATION_CONTEXT(3)
GLOBAL_UNCERTAINTY_ASSIGNED_CONTEXT((#16819))
GLOBAL_UNIT_ASSIGNED_CONTEXT((#16912,#16914,#16915))
REPRESENTATION_CONTEXT('','3D')
);
#16879=(
GEOMETRIC_REPRESENTATION_CONTEXT(3)
GLOBAL_UNCERTAINTY_ASSIGNED_CONTEXT((#16820))
GLOBAL_UNIT_ASSIGNED_CONTEXT((#16912,#16914,#16915))
REPRESENTATION_CONTEXT('','3D')
);
#16880=(
GEOMETRIC_REPRESENTATION_CONTEXT(3)
GLOBAL_UNCERTAINTY_ASSIGNED_CONTEXT((#16821))
GLOBAL_UNIT_ASSIGNED_CONTEXT((#16912,#16914,#16915))
REPRESENTATION_CONTEXT('','3D')
);
#16881=(
GEOMETRIC_REPRESENTATION_CONTEXT(3)
GLOBAL_UNCERTAINTY_ASSIGNED_CONTEXT((#16822))
GLOBAL_UNIT_ASSIGNED_CONTEXT((#16912,#16914,#16915))
REPRESENTATION_CONTEXT('','3D')
);
#16882=(
GEOMETRIC_REPRESENTATION_CONTEXT(3)
GLOBAL_UNCERTAINTY_ASSIGNED_CONTEXT((#16823))
GLOBAL_UNIT_ASSIGNED_CONTEXT((#16912,#16914,#16915))
REPRESENTATION_CONTEXT('','3D')
);
#16883=(
GEOMETRIC_REPRESENTATION_CONTEXT(3)
GLOBAL_UNCERTAINTY_ASSIGNED_CONTEXT((#16824))
GLOBAL_UNIT_ASSIGNED_CONTEXT((#16912,#16914,#16915))
REPRESENTATION_CONTEXT('','3D')
);
#16884=(
GEOMETRIC_REPRESENTATION_CONTEXT(3)
GLOBAL_UNCERTAINTY_ASSIGNED_CONTEXT((#16825))
GLOBAL_UNIT_ASSIGNED_CONTEXT((#16912,#16914,#16915))
REPRESENTATION_CONTEXT('','3D')
);
#16885=(
GEOMETRIC_REPRESENTATION_CONTEXT(3)
GLOBAL_UNCERTAINTY_ASSIGNED_CONTEXT((#16826))
GLOBAL_UNIT_ASSIGNED_CONTEXT((#16912,#16914,#16915))
REPRESENTATION_CONTEXT('','3D')
);
#16886=(
GEOMETRIC_REPRESENTATION_CONTEXT(3)
GLOBAL_UNCERTAINTY_ASSIGNED_CONTEXT((#16827))
GLOBAL_UNIT_ASSIGNED_CONTEXT((#16912,#16914,#16915))
REPRESENTATION_CONTEXT('','3D')
);
#16887=(
GEOMETRIC_REPRESENTATION_CONTEXT(3)
GLOBAL_UNCERTAINTY_ASSIGNED_CONTEXT((#16828))
GLOBAL_UNIT_ASSIGNED_CONTEXT((#16912,#16914,#16915))
REPRESENTATION_CONTEXT('','3D')
);
#16888=(
GEOMETRIC_REPRESENTATION_CONTEXT(3)
GLOBAL_UNCERTAINTY_ASSIGNED_CONTEXT((#16829))
GLOBAL_UNIT_ASSIGNED_CONTEXT((#16912,#16914,#16915))
REPRESENTATION_CONTEXT('','3D')
);
#16889=(
GEOMETRIC_REPRESENTATION_CONTEXT(3)
GLOBAL_UNCERTAINTY_ASSIGNED_CONTEXT((#16830))
GLOBAL_UNIT_ASSIGNED_CONTEXT((#16912,#16914,#16915))
REPRESENTATION_CONTEXT('','3D')
);
#16890=(
GEOMETRIC_REPRESENTATION_CONTEXT(3)
GLOBAL_UNCERTAINTY_ASSIGNED_CONTEXT((#16831))
GLOBAL_UNIT_ASSIGNED_CONTEXT((#16912,#16914,#16915))
REPRESENTATION_CONTEXT('','3D')
);
#16891=(
GEOMETRIC_REPRESENTATION_CONTEXT(3)
GLOBAL_UNCERTAINTY_ASSIGNED_CONTEXT((#16832))
GLOBAL_UNIT_ASSIGNED_CONTEXT((#16912,#16914,#16915))
REPRESENTATION_CONTEXT('','3D')
);
#16892=(
GEOMETRIC_REPRESENTATION_CONTEXT(3)
GLOBAL_UNCERTAINTY_ASSIGNED_CONTEXT((#16833))
GLOBAL_UNIT_ASSIGNED_CONTEXT((#16912,#16914,#16915))
REPRESENTATION_CONTEXT('','3D')
);
#16893=(
GEOMETRIC_REPRESENTATION_CONTEXT(3)
GLOBAL_UNCERTAINTY_ASSIGNED_CONTEXT((#16834))
GLOBAL_UNIT_ASSIGNED_CONTEXT((#16912,#16914,#16915))
REPRESENTATION_CONTEXT('','3D')
);
#16894=(
GEOMETRIC_REPRESENTATION_CONTEXT(3)
GLOBAL_UNCERTAINTY_ASSIGNED_CONTEXT((#16835))
GLOBAL_UNIT_ASSIGNED_CONTEXT((#16912,#16914,#16915))
REPRESENTATION_CONTEXT('','3D')
);
#16895=(
GEOMETRIC_REPRESENTATION_CONTEXT(3)
GLOBAL_UNCERTAINTY_ASSIGNED_CONTEXT((#16836))
GLOBAL_UNIT_ASSIGNED_CONTEXT((#16912,#16914,#16915))
REPRESENTATION_CONTEXT('','3D')
);
#16896=(
GEOMETRIC_REPRESENTATION_CONTEXT(3)
GLOBAL_UNCERTAINTY_ASSIGNED_CONTEXT((#16837))
GLOBAL_UNIT_ASSIGNED_CONTEXT((#16912,#16914,#16915))
REPRESENTATION_CONTEXT('','3D')
);
#16897=(
GEOMETRIC_REPRESENTATION_CONTEXT(3)
GLOBAL_UNCERTAINTY_ASSIGNED_CONTEXT((#16838))
GLOBAL_UNIT_ASSIGNED_CONTEXT((#16912,#16914,#16915))
REPRESENTATION_CONTEXT('','3D')
);
#16898=(
GEOMETRIC_REPRESENTATION_CONTEXT(3)
GLOBAL_UNCERTAINTY_ASSIGNED_CONTEXT((#16839))
GLOBAL_UNIT_ASSIGNED_CONTEXT((#16912,#16914,#16915))
REPRESENTATION_CONTEXT('','3D')
);
#16899=(
GEOMETRIC_REPRESENTATION_CONTEXT(3)
GLOBAL_UNCERTAINTY_ASSIGNED_CONTEXT((#16840))
GLOBAL_UNIT_ASSIGNED_CONTEXT((#16912,#16914,#16915))
REPRESENTATION_CONTEXT('','3D')
);
#16900=(
GEOMETRIC_REPRESENTATION_CONTEXT(3)
GLOBAL_UNCERTAINTY_ASSIGNED_CONTEXT((#16841))
GLOBAL_UNIT_ASSIGNED_CONTEXT((#16912,#16914,#16915))
REPRESENTATION_CONTEXT('','3D')
);
#16901=(
GEOMETRIC_REPRESENTATION_CONTEXT(3)
GLOBAL_UNCERTAINTY_ASSIGNED_CONTEXT((#16842))
GLOBAL_UNIT_ASSIGNED_CONTEXT((#16912,#16914,#16915))
REPRESENTATION_CONTEXT('','3D')
);
#16902=(
GEOMETRIC_REPRESENTATION_CONTEXT(3)
GLOBAL_UNCERTAINTY_ASSIGNED_CONTEXT((#16843))
GLOBAL_UNIT_ASSIGNED_CONTEXT((#16912,#16914,#16915))
REPRESENTATION_CONTEXT('','3D')
);
#16903=(
GEOMETRIC_REPRESENTATION_CONTEXT(3)
GLOBAL_UNCERTAINTY_ASSIGNED_CONTEXT((#16844))
GLOBAL_UNIT_ASSIGNED_CONTEXT((#16912,#16914,#16915))
REPRESENTATION_CONTEXT('','3D')
);
#16904=(
GEOMETRIC_REPRESENTATION_CONTEXT(3)
GLOBAL_UNCERTAINTY_ASSIGNED_CONTEXT((#16845))
GLOBAL_UNIT_ASSIGNED_CONTEXT((#16912,#16914,#16915))
REPRESENTATION_CONTEXT('','3D')
);
#16905=(
GEOMETRIC_REPRESENTATION_CONTEXT(3)
GLOBAL_UNCERTAINTY_ASSIGNED_CONTEXT((#16846))
GLOBAL_UNIT_ASSIGNED_CONTEXT((#16912,#16914,#16915))
REPRESENTATION_CONTEXT('','3D')
);
#16906=(
GEOMETRIC_REPRESENTATION_CONTEXT(3)
GLOBAL_UNCERTAINTY_ASSIGNED_CONTEXT((#16847))
GLOBAL_UNIT_ASSIGNED_CONTEXT((#16912,#16914,#16915))
REPRESENTATION_CONTEXT('','3D')
);
#16907=(
GEOMETRIC_REPRESENTATION_CONTEXT(3)
GLOBAL_UNCERTAINTY_ASSIGNED_CONTEXT((#16848))
GLOBAL_UNIT_ASSIGNED_CONTEXT((#16912,#16914,#16915))
REPRESENTATION_CONTEXT('','3D')
);
#16908=(
GEOMETRIC_REPRESENTATION_CONTEXT(3)
GLOBAL_UNCERTAINTY_ASSIGNED_CONTEXT((#16849))
GLOBAL_UNIT_ASSIGNED_CONTEXT((#16912,#16914,#16915))
REPRESENTATION_CONTEXT('','3D')
);
#16909=(
GEOMETRIC_REPRESENTATION_CONTEXT(3)
GLOBAL_UNCERTAINTY_ASSIGNED_CONTEXT((#16850))
GLOBAL_UNIT_ASSIGNED_CONTEXT((#16912,#16914,#16915))
REPRESENTATION_CONTEXT('','3D')
);
#16910=(
GEOMETRIC_REPRESENTATION_CONTEXT(3)
GLOBAL_UNCERTAINTY_ASSIGNED_CONTEXT((#16851))
GLOBAL_UNIT_ASSIGNED_CONTEXT((#16912,#16914,#16915))
REPRESENTATION_CONTEXT('','3D')
);
#16911=(
GEOMETRIC_REPRESENTATION_CONTEXT(3)
GLOBAL_UNCERTAINTY_ASSIGNED_CONTEXT((#16852))
GLOBAL_UNIT_ASSIGNED_CONTEXT((#16912,#16914,#16915))
REPRESENTATION_CONTEXT('','3D')
);
#16912=(
LENGTH_UNIT()
NAMED_UNIT(*)
SI_UNIT(.CENTI.,.METRE.)
);
#16913=(
LENGTH_UNIT()
NAMED_UNIT(*)
SI_UNIT($,.METRE.)
);
#16914=(
NAMED_UNIT(*)
PLANE_ANGLE_UNIT()
SI_UNIT($,.RADIAN.)
);
#16915=(
NAMED_UNIT(*)
SI_UNIT($,.STERADIAN.)
SOLID_ANGLE_UNIT()
);
#16916=SHAPE_DEFINITION_REPRESENTATION(#16974,#17124);
#16917=SHAPE_DEFINITION_REPRESENTATION(#16975,#17125);
#16918=SHAPE_DEFINITION_REPRESENTATION(#16976,#17126);
#16919=SHAPE_DEFINITION_REPRESENTATION(#16977,#17127);
#16920=SHAPE_DEFINITION_REPRESENTATION(#16978,#17128);
#16921=SHAPE_DEFINITION_REPRESENTATION(#16979,#17129);
#16922=SHAPE_DEFINITION_REPRESENTATION(#16980,#17130);
#16923=SHAPE_DEFINITION_REPRESENTATION(#16981,#17131);
#16924=SHAPE_DEFINITION_REPRESENTATION(#16982,#17132);
#16925=SHAPE_DEFINITION_REPRESENTATION(#16983,#17133);
#16926=SHAPE_DEFINITION_REPRESENTATION(#16984,#17134);
#16927=SHAPE_DEFINITION_REPRESENTATION(#16985,#17135);
#16928=SHAPE_DEFINITION_REPRESENTATION(#16986,#17136);
#16929=SHAPE_DEFINITION_REPRESENTATION(#16987,#17137);
#16930=SHAPE_DEFINITION_REPRESENTATION(#16988,#17138);
#16931=SHAPE_DEFINITION_REPRESENTATION(#16991,#17139);
#16932=SHAPE_DEFINITION_REPRESENTATION(#16992,#17140);
#16933=SHAPE_DEFINITION_REPRESENTATION(#16993,#17141);
#16934=SHAPE_DEFINITION_REPRESENTATION(#16994,#17142);
#16935=SHAPE_DEFINITION_REPRESENTATION(#16995,#17143);
#16936=SHAPE_DEFINITION_REPRESENTATION(#16996,#17144);
#16937=SHAPE_DEFINITION_REPRESENTATION(#16997,#17145);
#16938=SHAPE_DEFINITION_REPRESENTATION(#16998,#17146);
#16939=SHAPE_DEFINITION_REPRESENTATION(#16999,#17147);
#16940=SHAPE_DEFINITION_REPRESENTATION(#17000,#17148);
#16941=SHAPE_DEFINITION_REPRESENTATION(#17001,#17149);
#16942=SHAPE_DEFINITION_REPRESENTATION(#17002,#17150);
#16943=SHAPE_DEFINITION_REPRESENTATION(#17003,#17151);
#16944=SHAPE_DEFINITION_REPRESENTATION(#17004,#17152);
#16945=SHAPE_DEFINITION_REPRESENTATION(#17005,#17153);
#16946=SHAPE_DEFINITION_REPRESENTATION(#17006,#17154);
#16947=SHAPE_DEFINITION_REPRESENTATION(#17007,#17155);
#16948=SHAPE_DEFINITION_REPRESENTATION(#17008,#17156);
#16949=SHAPE_DEFINITION_REPRESENTATION(#17009,#17157);
#16950=SHAPE_DEFINITION_REPRESENTATION(#17010,#17158);
#16951=SHAPE_DEFINITION_REPRESENTATION(#17011,#17159);
#16952=SHAPE_DEFINITION_REPRESENTATION(#17012,#17160);
#16953=SHAPE_DEFINITION_REPRESENTATION(#17013,#17161);
#16954=SHAPE_DEFINITION_REPRESENTATION(#17014,#17162);
#16955=SHAPE_DEFINITION_REPRESENTATION(#17015,#17163);
#16956=SHAPE_DEFINITION_REPRESENTATION(#17016,#17164);
#16957=SHAPE_DEFINITION_REPRESENTATION(#17017,#17165);
#16958=SHAPE_DEFINITION_REPRESENTATION(#17018,#17166);
#16959=SHAPE_DEFINITION_REPRESENTATION(#17031,#17167);
#16960=SHAPE_DEFINITION_REPRESENTATION(#17032,#17168);
#16961=SHAPE_DEFINITION_REPRESENTATION(#17033,#17169);
#16962=SHAPE_DEFINITION_REPRESENTATION(#17034,#17170);
#16963=SHAPE_DEFINITION_REPRESENTATION(#17035,#17171);
#16964=SHAPE_DEFINITION_REPRESENTATION(#17036,#17172);
#16965=SHAPE_DEFINITION_REPRESENTATION(#17037,#17173);
#16966=SHAPE_DEFINITION_REPRESENTATION(#17038,#17174);
#16967=SHAPE_DEFINITION_REPRESENTATION(#17039,#17175);
#16968=SHAPE_DEFINITION_REPRESENTATION(#17040,#17176);
#16969=SHAPE_DEFINITION_REPRESENTATION(#17041,#17177);
#16970=SHAPE_DEFINITION_REPRESENTATION(#17045,#17178);
#16971=SHAPE_DEFINITION_REPRESENTATION(#17046,#17179);
#16972=SHAPE_DEFINITION_REPRESENTATION(#17047,#17180);
#16973=SHAPE_DEFINITION_REPRESENTATION(#17085,#17181);
#16974=PRODUCT_DEFINITION_SHAPE('',$,#17183);
#16975=PRODUCT_DEFINITION_SHAPE('',$,#17184);
#16976=PRODUCT_DEFINITION_SHAPE('',$,#17185);
#16977=PRODUCT_DEFINITION_SHAPE('',$,#17186);
#16978=PRODUCT_DEFINITION_SHAPE('',$,#17187);
#16979=PRODUCT_DEFINITION_SHAPE('',$,#17188);
#16980=PRODUCT_DEFINITION_SHAPE('',$,#17189);
#16981=PRODUCT_DEFINITION_SHAPE('',$,#17190);
#16982=PRODUCT_DEFINITION_SHAPE('',$,#17191);
#16983=PRODUCT_DEFINITION_SHAPE('',$,#17192);
#16984=PRODUCT_DEFINITION_SHAPE('',$,#17193);
#16985=PRODUCT_DEFINITION_SHAPE('',$,#17194);
#16986=PRODUCT_DEFINITION_SHAPE('',$,#17195);
#16987=PRODUCT_DEFINITION_SHAPE('',$,#17196);
#16988=PRODUCT_DEFINITION_SHAPE('',$,#17197);
#16989=PRODUCT_DEFINITION_SHAPE($,$,#323);
#16990=PRODUCT_DEFINITION_SHAPE($,$,#324);
#16991=PRODUCT_DEFINITION_SHAPE('',$,#17198);
#16992=PRODUCT_DEFINITION_SHAPE('',$,#17199);
#16993=PRODUCT_DEFINITION_SHAPE('',$,#17200);
#16994=PRODUCT_DEFINITION_SHAPE('',$,#17201);
#16995=PRODUCT_DEFINITION_SHAPE('',$,#17202);
#16996=PRODUCT_DEFINITION_SHAPE('',$,#17203);
#16997=PRODUCT_DEFINITION_SHAPE('',$,#17204);
#16998=PRODUCT_DEFINITION_SHAPE('',$,#17205);
#16999=PRODUCT_DEFINITION_SHAPE('',$,#17206);
#17000=PRODUCT_DEFINITION_SHAPE('',$,#17207);
#17001=PRODUCT_DEFINITION_SHAPE('',$,#17208);
#17002=PRODUCT_DEFINITION_SHAPE('',$,#17209);
#17003=PRODUCT_DEFINITION_SHAPE('',$,#17210);
#17004=PRODUCT_DEFINITION_SHAPE('',$,#17211);
#17005=PRODUCT_DEFINITION_SHAPE('',$,#17212);
#17006=PRODUCT_DEFINITION_SHAPE('',$,#17213);
#17007=PRODUCT_DEFINITION_SHAPE('',$,#17214);
#17008=PRODUCT_DEFINITION_SHAPE('',$,#17215);
#17009=PRODUCT_DEFINITION_SHAPE('',$,#17216);
#17010=PRODUCT_DEFINITION_SHAPE('',$,#17217);
#17011=PRODUCT_DEFINITION_SHAPE('',$,#17218);
#17012=PRODUCT_DEFINITION_SHAPE('',$,#17219);
#17013=PRODUCT_DEFINITION_SHAPE('',$,#17220);
#17014=PRODUCT_DEFINITION_SHAPE('',$,#17221);
#17015=PRODUCT_DEFINITION_SHAPE('',$,#17222);
#17016=PRODUCT_DEFINITION_SHAPE('',$,#17223);
#17017=PRODUCT_DEFINITION_SHAPE('',$,#17224);
#17018=PRODUCT_DEFINITION_SHAPE('',$,#17225);
#17019=PRODUCT_DEFINITION_SHAPE($,$,#325);
#17020=PRODUCT_DEFINITION_SHAPE($,$,#326);
#17021=PRODUCT_DEFINITION_SHAPE($,$,#327);
#17022=PRODUCT_DEFINITION_SHAPE($,$,#328);
#17023=PRODUCT_DEFINITION_SHAPE($,$,#329);
#17024=PRODUCT_DEFINITION_SHAPE($,$,#330);
#17025=PRODUCT_DEFINITION_SHAPE($,$,#331);
#17026=PRODUCT_DEFINITION_SHAPE($,$,#332);
#17027=PRODUCT_DEFINITION_SHAPE($,$,#333);
#17028=PRODUCT_DEFINITION_SHAPE($,$,#334);
#17029=PRODUCT_DEFINITION_SHAPE($,$,#335);
#17030=PRODUCT_DEFINITION_SHAPE($,$,#336);
#17031=PRODUCT_DEFINITION_SHAPE('',$,#17226);
#17032=PRODUCT_DEFINITION_SHAPE('',$,#17227);
#17033=PRODUCT_DEFINITION_SHAPE('',$,#17228);
#17034=PRODUCT_DEFINITION_SHAPE('',$,#17229);
#17035=PRODUCT_DEFINITION_SHAPE('',$,#17230);
#17036=PRODUCT_DEFINITION_SHAPE('',$,#17231);
#17037=PRODUCT_DEFINITION_SHAPE('',$,#17232);
#17038=PRODUCT_DEFINITION_SHAPE('',$,#17233);
#17039=PRODUCT_DEFINITION_SHAPE('',$,#17234);
#17040=PRODUCT_DEFINITION_SHAPE('',$,#17235);
#17041=PRODUCT_DEFINITION_SHAPE('',$,#17236);
#17042=PRODUCT_DEFINITION_SHAPE($,$,#337);
#17043=PRODUCT_DEFINITION_SHAPE($,$,#338);
#17044=PRODUCT_DEFINITION_SHAPE($,$,#339);
#17045=PRODUCT_DEFINITION_SHAPE('',$,#17237);
#17046=PRODUCT_DEFINITION_SHAPE('',$,#17238);
#17047=PRODUCT_DEFINITION_SHAPE('',$,#17239);
#17048=PRODUCT_DEFINITION_SHAPE($,$,#340);
#17049=PRODUCT_DEFINITION_SHAPE($,$,#341);
#17050=PRODUCT_DEFINITION_SHAPE($,$,#342);
#17051=PRODUCT_DEFINITION_SHAPE($,$,#343);
#17052=PRODUCT_DEFINITION_SHAPE($,$,#344);
#17053=PRODUCT_DEFINITION_SHAPE($,$,#345);
#17054=PRODUCT_DEFINITION_SHAPE($,$,#346);
#17055=PRODUCT_DEFINITION_SHAPE($,$,#347);
#17056=PRODUCT_DEFINITION_SHAPE($,$,#348);
#17057=PRODUCT_DEFINITION_SHAPE($,$,#349);
#17058=PRODUCT_DEFINITION_SHAPE($,$,#350);
#17059=PRODUCT_DEFINITION_SHAPE($,$,#351);
#17060=PRODUCT_DEFINITION_SHAPE($,$,#352);
#17061=PRODUCT_DEFINITION_SHAPE($,$,#353);
#17062=PRODUCT_DEFINITION_SHAPE($,$,#354);
#17063=PRODUCT_DEFINITION_SHAPE($,$,#355);
#17064=PRODUCT_DEFINITION_SHAPE($,$,#356);
#17065=PRODUCT_DEFINITION_SHAPE($,$,#357);
#17066=PRODUCT_DEFINITION_SHAPE($,$,#358);
#17067=PRODUCT_DEFINITION_SHAPE($,$,#359);
#17068=PRODUCT_DEFINITION_SHAPE($,$,#360);
#17069=PRODUCT_DEFINITION_SHAPE($,$,#361);
#17070=PRODUCT_DEFINITION_SHAPE($,$,#362);
#17071=PRODUCT_DEFINITION_SHAPE($,$,#363);
#17072=PRODUCT_DEFINITION_SHAPE($,$,#364);
#17073=PRODUCT_DEFINITION_SHAPE($,$,#365);
#17074=PRODUCT_DEFINITION_SHAPE($,$,#366);
#17075=PRODUCT_DEFINITION_SHAPE($,$,#367);
#17076=PRODUCT_DEFINITION_SHAPE($,$,#368);
#17077=PRODUCT_DEFINITION_SHAPE($,$,#369);
#17078=PRODUCT_DEFINITION_SHAPE($,$,#370);
#17079=PRODUCT_DEFINITION_SHAPE($,$,#371);
#17080=PRODUCT_DEFINITION_SHAPE($,$,#372);
#17081=PRODUCT_DEFINITION_SHAPE($,$,#373);
#17082=PRODUCT_DEFINITION_SHAPE($,$,#374);
#17083=PRODUCT_DEFINITION_SHAPE($,$,#375);
#17084=PRODUCT_DEFINITION_SHAPE($,$,#376);
#17085=PRODUCT_DEFINITION_SHAPE('',$,#17240);
#17086=PRODUCT_DEFINITION_SHAPE($,$,#377);
#17087=PRODUCT_DEFINITION_SHAPE($,$,#378);
#17088=PRODUCT_DEFINITION_SHAPE($,$,#379);
#17089=PRODUCT_DEFINITION_SHAPE($,$,#380);
#17090=PRODUCT_DEFINITION_SHAPE($,$,#381);
#17091=PRODUCT_DEFINITION_SHAPE($,$,#382);
#17092=PRODUCT_DEFINITION_SHAPE($,$,#383);
#17093=PRODUCT_DEFINITION_SHAPE($,$,#384);
#17094=PRODUCT_DEFINITION_SHAPE($,$,#385);
#17095=PRODUCT_DEFINITION_SHAPE($,$,#386);
#17096=PRODUCT_DEFINITION_SHAPE($,$,#387);
#17097=PRODUCT_DEFINITION_SHAPE($,$,#388);
#17098=PRODUCT_DEFINITION_SHAPE($,$,#389);
#17099=PRODUCT_DEFINITION_SHAPE($,$,#390);
#17100=PRODUCT_DEFINITION_SHAPE($,$,#391);
#17101=PRODUCT_DEFINITION_SHAPE($,$,#392);
#17102=PRODUCT_DEFINITION_SHAPE($,$,#393);
#17103=PRODUCT_DEFINITION_SHAPE($,$,#394);
#17104=PRODUCT_DEFINITION_SHAPE($,$,#395);
#17105=PRODUCT_DEFINITION_SHAPE($,$,#396);
#17106=PRODUCT_DEFINITION_SHAPE($,$,#397);
#17107=PRODUCT_DEFINITION_SHAPE($,$,#398);
#17108=PRODUCT_DEFINITION_SHAPE($,$,#399);
#17109=PRODUCT_DEFINITION_SHAPE($,$,#400);
#17110=PRODUCT_DEFINITION_SHAPE($,$,#401);
#17111=PRODUCT_DEFINITION_SHAPE($,$,#402);
#17112=PRODUCT_DEFINITION_SHAPE($,$,#403);
#17113=PRODUCT_DEFINITION_SHAPE($,$,#404);
#17114=PRODUCT_DEFINITION_SHAPE($,$,#405);
#17115=PRODUCT_DEFINITION_SHAPE($,$,#406);
#17116=PRODUCT_DEFINITION_SHAPE($,$,#407);
#17117=PRODUCT_DEFINITION_SHAPE($,$,#408);
#17118=PRODUCT_DEFINITION_SHAPE($,$,#409);
#17119=PRODUCT_DEFINITION_SHAPE($,$,#410);
#17120=PRODUCT_DEFINITION_SHAPE($,$,#411);
#17121=PRODUCT_DEFINITION_SHAPE($,$,#412);
#17122=PRODUCT_DEFINITION_SHAPE($,$,#413);
#17123=PRODUCT_DEFINITION_SHAPE($,$,#414);
#17124=SHAPE_REPRESENTATION('',(#9493,#10562,#10563,#10564,#10565),#16853);
#17125=SHAPE_REPRESENTATION('',(#9494,#10467,#10468,#10469,#10470,#10471,
#10472,#10473,#10474,#10475,#10476,#10477,#10478,#10479,#10480,#10481,#10482,
#10483,#10484,#10485,#10486,#10487,#10488,#10489,#10490,#10491,#10492,#10493,
#10494,#10495,#10496,#10497,#10498,#10499,#10500,#10501,#10502,#10503),
#16854);
#17126=SHAPE_REPRESENTATION('',(#9495),#16855);
#17127=SHAPE_REPRESENTATION('',(#9538),#16856);
#17128=SHAPE_REPRESENTATION('',(#9581),#16857);
#17129=SHAPE_REPRESENTATION('',(#9590),#16858);
#17130=SHAPE_REPRESENTATION('',(#9599),#16859);
#17131=SHAPE_REPRESENTATION('',(#9642),#16860);
#17132=SHAPE_REPRESENTATION('',(#9651),#16861);
#17133=SHAPE_REPRESENTATION('',(#9660),#16862);
#17134=SHAPE_REPRESENTATION('',(#9711),#16863);
#17135=SHAPE_REPRESENTATION('',(#9718),#16864);
#17136=SHAPE_REPRESENTATION('',(#9725,#9795,#9796),#16865);
#17137=SHAPE_REPRESENTATION('',(#9726),#16866);
#17138=SHAPE_REPRESENTATION('',(#9767),#16867);
#17139=SHAPE_REPRESENTATION('',(#9797),#16868);
#17140=SHAPE_REPRESENTATION('',(#9806),#16869);
#17141=SHAPE_REPRESENTATION('',(#9830),#16870);
#17142=SHAPE_REPRESENTATION('',(#9873),#16871);
#17143=SHAPE_REPRESENTATION('',(#9899,#10528,#10529,#10530,#10531,#10532,
#10533,#10534,#10535,#10536,#10537,#10538,#10539,#10540,#10541),#16872);
#17144=SHAPE_REPRESENTATION('',(#9900),#16873);
#17145=SHAPE_REPRESENTATION('',(#9912),#16874);
#17146=SHAPE_REPRESENTATION('',(#9927),#16875);
#17147=SHAPE_REPRESENTATION('',(#9942),#16876);
#17148=SHAPE_REPRESENTATION('',(#9951),#16877);
#17149=SHAPE_REPRESENTATION('',(#9983),#16878);
#17150=SHAPE_REPRESENTATION('',(#9997),#16879);
#17151=SHAPE_REPRESENTATION('',(#10006),#16880);
#17152=SHAPE_REPRESENTATION('',(#10015),#16881);
#17153=SHAPE_REPRESENTATION('',(#10024),#16882);
#17154=SHAPE_REPRESENTATION('',(#10035),#16883);
#17155=SHAPE_REPRESENTATION('',(#10052,#10240,#10241,#10242,#10243,#10244,
#10245,#10246),#16884);
#17156=SHAPE_REPRESENTATION('',(#10053),#16885);
#17157=SHAPE_REPRESENTATION('',(#10070),#16886);
#17158=SHAPE_REPRESENTATION('',(#10079),#16887);
#17159=SHAPE_REPRESENTATION('',(#10088),#16888);
#17160=SHAPE_REPRESENTATION('',(#10097),#16889);
#17161=SHAPE_REPRESENTATION('',(#10106,#10235,#10236,#10237,#10238,#10239),
#16890);
#17162=SHAPE_REPRESENTATION('',(#10107),#16891);
#17163=SHAPE_REPRESENTATION('',(#10127),#16892);
#17164=SHAPE_REPRESENTATION('',(#10147),#16893);
#17165=SHAPE_REPRESENTATION('',(#10164),#16894);
#17166=SHAPE_REPRESENTATION('',(#10218),#16895);
#17167=SHAPE_REPRESENTATION('',(#10247,#10542,#10543,#10544,#10545,#10546,
#10547,#10548,#10549,#10550,#10551,#10552,#10553,#10554,#10555,#10556,#10557,
#10558,#10559,#10560,#10561),#16896);
#17168=SHAPE_REPRESENTATION('',(#10248),#16897);
#17169=SHAPE_REPRESENTATION('',(#10287),#16898);
#17170=SHAPE_REPRESENTATION('',(#10300),#16899);
#17171=SHAPE_REPRESENTATION('',(#10314),#16900);
#17172=SHAPE_REPRESENTATION('',(#10323),#16901);
#17173=SHAPE_REPRESENTATION('',(#10332),#16902);
#17174=SHAPE_REPRESENTATION('',(#10341,#10403,#10404,#10405),#16903);
#17175=SHAPE_REPRESENTATION('',(#10342),#16904);
#17176=SHAPE_REPRESENTATION('',(#10381),#16905);
#17177=SHAPE_REPRESENTATION('',(#10392),#16906);
#17178=SHAPE_REPRESENTATION('',(#10406),#16907);
#17179=SHAPE_REPRESENTATION('',(#10430),#16908);
#17180=SHAPE_REPRESENTATION('',(#10441),#16909);
#17181=SHAPE_REPRESENTATION('',(#10504),#16910);
#17182=PRODUCT_DEFINITION_CONTEXT('part definition',#17358,'design');
#17183=PRODUCT_DEFINITION('PAT-034','PAT-034',#17241,
#17182);
#17184=PRODUCT_DEFINITION('Bearing and guide frame',
'Bearing and guide frame',#17242,#17182);
#17185=PRODUCT_DEFINITION('Base','Base',#17243,#17182);
#17186=PRODUCT_DEFINITION('Bearing pedestal','Bearing pedestal',#17244,
#17182);
#17187=PRODUCT_DEFINITION('Bearing bolt reducer','Bearing bolt reducer',
#17245,#17182);
#17188=PRODUCT_DEFINITION('Bearing bolt reducer (1)',
'Bearing bolt reducer (1)',#17246,#17182);
#17189=PRODUCT_DEFINITION('Bearing pedestal (1)','Bearing pedestal (1)',#17247,
#17182);
#17190=PRODUCT_DEFINITION('Bearing bolt reducer (2)',
'Bearing bolt reducer (2)',#17248,#17182);
#17191=PRODUCT_DEFINITION('Bearing bolt reducer (3)',
'Bearing bolt reducer (3)',#17249,#17182);
#17192=PRODUCT_DEFINITION('Rail pedestal','Rail pedestal',#17250,#17182);
#17193=PRODUCT_DEFINITION('Foot strip','Foot strip',#17251,#17182);
#17194=PRODUCT_DEFINITION('Foot strip (1)','Foot strip (1)',#17252,#17182);
#17195=PRODUCT_DEFINITION('Pillow Block Bearing - 20 mm Bore',
'Pillow Block Bearing - 20 mm Bore',#17253,#17182);
#17196=PRODUCT_DEFINITION('Housing','Housing',#17254,#17182);
#17197=PRODUCT_DEFINITION('Insert bearing','Insert bearing',#17255,#17182);
#17198=PRODUCT_DEFINITION('Flat Washer - M8','Flat Washer - M8',#17256,
#17182);
#17199=PRODUCT_DEFINITION('M8x25 Bolt','M8x25 Bolt',#17257,#17182);
#17200=PRODUCT_DEFINITION('Linear Guide Rail - 15 mm, 220 mm Long',
'Linear Guide Rail - 15 mm, 220 mm Long',#17258,#17182);
#17201=PRODUCT_DEFINITION('Cap Screw - M4x16','Cap Screw - M4x16',#17259,
#17182);
#17202=PRODUCT_DEFINITION('Flywheel and crank','Flywheel and crank',#17260,
#17182);
#17203=PRODUCT_DEFINITION('Flywheel shaft','Flywheel shaft',#17261,#17182);
#17204=PRODUCT_DEFINITION('Shaft collar','Shaft collar',#17262,#17182);
#17205=PRODUCT_DEFINITION('Shaft collar (1)','Shaft collar (1)',#17263,#17182);
#17206=PRODUCT_DEFINITION('Rear bearing spacer','Rear bearing spacer',#17264,
#17182);
#17207=PRODUCT_DEFINITION('Flywheel','Flywheel',#17265,#17182);
#17208=PRODUCT_DEFINITION('Crank pin','Crank pin',#17266,#17182);
#17209=PRODUCT_DEFINITION('Pin spacer 15 mm','Pin spacer 15 mm',#17267,
#17182);
#17210=PRODUCT_DEFINITION('Pin spacer 4 mm','Pin spacer 4 mm',#17268,#17182);
#17211=PRODUCT_DEFINITION('Pin keeper','Pin keeper',#17269,#17182);
#17212=PRODUCT_DEFINITION('Key 6x6x20','Key 6x6x20',#17270,#17182);
#17213=PRODUCT_DEFINITION('Socket Set Screw - M5x8',
'Socket Set Screw - M5x8',#17271,#17182);
#17214=PRODUCT_DEFINITION('Connecting rod (1)','Connecting rod (1)',#17272,
#17182);
#17215=PRODUCT_DEFINITION('Connecting rod','Connecting rod',#17273,#17182);
#17216=PRODUCT_DEFINITION('Rod bearing retainer','Rod bearing retainer',
#17274,#17182);
#17217=PRODUCT_DEFINITION('Rod bearing retainer (1)',
'Rod bearing retainer (1)',#17275,#17182);
#17218=PRODUCT_DEFINITION('Rod bearing retainer (2)',
'Rod bearing retainer (2)',#17276,#17182);
#17219=PRODUCT_DEFINITION('Rod bearing retainer (3)',
'Rod bearing retainer (3)',#17277,#17182);
#17220=PRODUCT_DEFINITION('Sealed Ball Bearing - 10 x 30 x 9 mm',
'Sealed Ball Bearing - 10 x 30 x 9 mm',#17278,#17182);
#17221=PRODUCT_DEFINITION('Inner ring','Inner ring',#17279,#17182);
#17222=PRODUCT_DEFINITION('Outer ring','Outer ring',#17280,#17182);
#17223=PRODUCT_DEFINITION('Balls','Balls',#17281,#17182);
#17224=PRODUCT_DEFINITION('Cage','Cage',#17282,#17182);
#17225=PRODUCT_DEFINITION('Seals 2RS','Seals 2RS',#17283,#17182);
#17226=PRODUCT_DEFINITION('Guided slider','Guided slider',#17284,#17182);
#17227=PRODUCT_DEFINITION('Specimen carriage','Specimen carriage',#17285,
#17182);
#17228=PRODUCT_DEFINITION('Specimen clamp jaw','Specimen clamp jaw',#17286,
#17182);
#17229=PRODUCT_DEFINITION('Slider pin','Slider pin',#17287,#17182);
#17230=PRODUCT_DEFINITION('Pin spacer 2 mm','Pin spacer 2 mm',#17288,#17182);
#17231=PRODUCT_DEFINITION('Pin spacer 4 mm (1)','Pin spacer 4 mm (1)',#17289,
#17182);
#17232=PRODUCT_DEFINITION('Pin keeper (1)','Pin keeper (1)',#17290,#17182);
#17233=PRODUCT_DEFINITION('Flanged Linear Guide Carriage - 15 mm',
'Flanged Linear Guide Carriage - 15 mm',#17291,#17182);
#17234=PRODUCT_DEFINITION('Block','Block',#17292,#17182);
#17235=PRODUCT_DEFINITION('End cap +','End cap +',#17293,#17182);
#17236=PRODUCT_DEFINITION('End cap','End cap',#17294,#17182);
#17237=PRODUCT_DEFINITION('M5x14 Cap Screw','M5x14 Cap Screw',#17295,#17182);
#17238=PRODUCT_DEFINITION('Flat Washer - M5','Flat Washer - M5',#17296,
#17182);
#17239=PRODUCT_DEFINITION('Cap Screw - M5x20','Cap Screw - M5x20',#17297,
#17182);
#17240=PRODUCT_DEFINITION('M4x10 Cap Screw','M4x10 Cap Screw',#17298,#17182);
#17241=PRODUCT_DEFINITION_FORMATION('',$,#17360);
#17242=PRODUCT_DEFINITION_FORMATION('',$,#17361);
#17243=PRODUCT_DEFINITION_FORMATION('',$,#17362);
#17244=PRODUCT_DEFINITION_FORMATION('',$,#17363);
#17245=PRODUCT_DEFINITION_FORMATION('',$,#17364);
#17246=PRODUCT_DEFINITION_FORMATION('',$,#17365);
#17247=PRODUCT_DEFINITION_FORMATION('',$,#17366);
#17248=PRODUCT_DEFINITION_FORMATION('',$,#17367);
#17249=PRODUCT_DEFINITION_FORMATION('',$,#17368);
#17250=PRODUCT_DEFINITION_FORMATION('',$,#17369);
#17251=PRODUCT_DEFINITION_FORMATION('',$,#17370);
#17252=PRODUCT_DEFINITION_FORMATION('',$,#17371);
#17253=PRODUCT_DEFINITION_FORMATION('',$,#17372);
#17254=PRODUCT_DEFINITION_FORMATION('',$,#17373);
#17255=PRODUCT_DEFINITION_FORMATION('',$,#17374);
#17256=PRODUCT_DEFINITION_FORMATION('',$,#17375);
#17257=PRODUCT_DEFINITION_FORMATION('',$,#17376);
#17258=PRODUCT_DEFINITION_FORMATION('',$,#17377);
#17259=PRODUCT_DEFINITION_FORMATION('',$,#17378);
#17260=PRODUCT_DEFINITION_FORMATION('',$,#17379);
#17261=PRODUCT_DEFINITION_FORMATION('',$,#17380);
#17262=PRODUCT_DEFINITION_FORMATION('',$,#17381);
#17263=PRODUCT_DEFINITION_FORMATION('',$,#17382);
#17264=PRODUCT_DEFINITION_FORMATION('',$,#17383);
#17265=PRODUCT_DEFINITION_FORMATION('',$,#17384);
#17266=PRODUCT_DEFINITION_FORMATION('',$,#17385);
#17267=PRODUCT_DEFINITION_FORMATION('',$,#17386);
#17268=PRODUCT_DEFINITION_FORMATION('',$,#17387);
#17269=PRODUCT_DEFINITION_FORMATION('',$,#17388);
#17270=PRODUCT_DEFINITION_FORMATION('',$,#17389);
#17271=PRODUCT_DEFINITION_FORMATION('',$,#17390);
#17272=PRODUCT_DEFINITION_FORMATION('',$,#17391);
#17273=PRODUCT_DEFINITION_FORMATION('',$,#17392);
#17274=PRODUCT_DEFINITION_FORMATION('',$,#17393);
#17275=PRODUCT_DEFINITION_FORMATION('',$,#17394);
#17276=PRODUCT_DEFINITION_FORMATION('',$,#17395);
#17277=PRODUCT_DEFINITION_FORMATION('',$,#17396);
#17278=PRODUCT_DEFINITION_FORMATION('',$,#17397);
#17279=PRODUCT_DEFINITION_FORMATION('',$,#17398);
#17280=PRODUCT_DEFINITION_FORMATION('',$,#17399);
#17281=PRODUCT_DEFINITION_FORMATION('',$,#17400);
#17282=PRODUCT_DEFINITION_FORMATION('',$,#17401);
#17283=PRODUCT_DEFINITION_FORMATION('',$,#17402);
#17284=PRODUCT_DEFINITION_FORMATION('',$,#17403);
#17285=PRODUCT_DEFINITION_FORMATION('',$,#17404);
#17286=PRODUCT_DEFINITION_FORMATION('',$,#17405);
#17287=PRODUCT_DEFINITION_FORMATION('',$,#17406);
#17288=PRODUCT_DEFINITION_FORMATION('',$,#17407);
#17289=PRODUCT_DEFINITION_FORMATION('',$,#17408);
#17290=PRODUCT_DEFINITION_FORMATION('',$,#17409);
#17291=PRODUCT_DEFINITION_FORMATION('',$,#17410);
#17292=PRODUCT_DEFINITION_FORMATION('',$,#17411);
#17293=PRODUCT_DEFINITION_FORMATION('',$,#17412);
#17294=PRODUCT_DEFINITION_FORMATION('',$,#17413);
#17295=PRODUCT_DEFINITION_FORMATION('',$,#17414);
#17296=PRODUCT_DEFINITION_FORMATION('',$,#17415);
#17297=PRODUCT_DEFINITION_FORMATION('',$,#17416);
#17298=PRODUCT_DEFINITION_FORMATION('',$,#17417);
#17299=PRODUCT_RELATED_PRODUCT_CATEGORY('PAT-034','PAT-034',(#17360));
#17300=PRODUCT_RELATED_PRODUCT_CATEGORY('Bearing and guide frame',
'Bearing and guide frame',(#17361));
#17301=PRODUCT_RELATED_PRODUCT_CATEGORY('Base','Base',(#17362));
#17302=PRODUCT_RELATED_PRODUCT_CATEGORY('Bearing pedestal',
'Bearing pedestal',(#17363));
#17303=PRODUCT_RELATED_PRODUCT_CATEGORY('Bearing bolt reducer',
'Bearing bolt reducer',(#17364));
#17304=PRODUCT_RELATED_PRODUCT_CATEGORY('Bearing bolt reducer (1)',
'Bearing bolt reducer (1)',(#17365));
#17305=PRODUCT_RELATED_PRODUCT_CATEGORY('Bearing pedestal (1)',
'Bearing pedestal (1)',(#17366));
#17306=PRODUCT_RELATED_PRODUCT_CATEGORY('Bearing bolt reducer (2)',
'Bearing bolt reducer (2)',(#17367));
#17307=PRODUCT_RELATED_PRODUCT_CATEGORY('Bearing bolt reducer (3)',
'Bearing bolt reducer (3)',(#17368));
#17308=PRODUCT_RELATED_PRODUCT_CATEGORY('Rail pedestal','Rail pedestal',
(#17369));
#17309=PRODUCT_RELATED_PRODUCT_CATEGORY('Foot strip','Foot strip',(#17370));
#17310=PRODUCT_RELATED_PRODUCT_CATEGORY('Foot strip (1)',
'Foot strip (1)',(#17371));
#17311=PRODUCT_RELATED_PRODUCT_CATEGORY(
'Pillow Block Bearing - 20 mm Bore','Pillow Block Bearing - 20 mm Bore',
(#17372));
#17312=PRODUCT_RELATED_PRODUCT_CATEGORY('Housing','Housing',(#17373));
#17313=PRODUCT_RELATED_PRODUCT_CATEGORY('Insert bearing',
'Insert bearing',(#17374));
#17314=PRODUCT_RELATED_PRODUCT_CATEGORY('Flat Washer - M8',
'Flat Washer - M8',(#17375));
#17315=PRODUCT_RELATED_PRODUCT_CATEGORY('M8x25 Bolt','M8x25 Bolt',(#17376));
#17316=PRODUCT_RELATED_PRODUCT_CATEGORY(
'Linear Guide Rail - 15 mm, 220 mm Long',
'Linear Guide Rail - 15 mm, 220 mm Long',(#17377));
#17317=PRODUCT_RELATED_PRODUCT_CATEGORY('Cap Screw - M4x16',
'Cap Screw - M4x16',(#17378));
#17318=PRODUCT_RELATED_PRODUCT_CATEGORY('Flywheel and crank',
'Flywheel and crank',(#17379));
#17319=PRODUCT_RELATED_PRODUCT_CATEGORY('Flywheel shaft',
'Flywheel shaft',(#17380));
#17320=PRODUCT_RELATED_PRODUCT_CATEGORY('Shaft collar','Shaft collar',(#17381));
#17321=PRODUCT_RELATED_PRODUCT_CATEGORY('Shaft collar (1)',
'Shaft collar (1)',(#17382));
#17322=PRODUCT_RELATED_PRODUCT_CATEGORY('Rear bearing spacer',
'Rear bearing spacer',(#17383));
#17323=PRODUCT_RELATED_PRODUCT_CATEGORY('Flywheel','Flywheel',(#17384));
#17324=PRODUCT_RELATED_PRODUCT_CATEGORY('Crank pin','Crank pin',(#17385));
#17325=PRODUCT_RELATED_PRODUCT_CATEGORY('Pin spacer 15 mm',
'Pin spacer 15 mm',(#17386));
#17326=PRODUCT_RELATED_PRODUCT_CATEGORY('Pin spacer 4 mm',
'Pin spacer 4 mm',(#17387));
#17327=PRODUCT_RELATED_PRODUCT_CATEGORY('Pin keeper','Pin keeper',(#17388));
#17328=PRODUCT_RELATED_PRODUCT_CATEGORY('Key 6x6x20','Key 6x6x20',(#17389));
#17329=PRODUCT_RELATED_PRODUCT_CATEGORY('Socket Set Screw - M5x8',
'Socket Set Screw - M5x8',(#17390));
#17330=PRODUCT_RELATED_PRODUCT_CATEGORY('Connecting rod (1)',
'Connecting rod (1)',(#17391));
#17331=PRODUCT_RELATED_PRODUCT_CATEGORY('Connecting rod',
'Connecting rod',(#17392));
#17332=PRODUCT_RELATED_PRODUCT_CATEGORY('Rod bearing retainer',
'Rod bearing retainer',(#17393));
#17333=PRODUCT_RELATED_PRODUCT_CATEGORY('Rod bearing retainer (1)',
'Rod bearing retainer (1)',(#17394));
#17334=PRODUCT_RELATED_PRODUCT_CATEGORY('Rod bearing retainer (2)',
'Rod bearing retainer (2)',(#17395));
#17335=PRODUCT_RELATED_PRODUCT_CATEGORY('Rod bearing retainer (3)',
'Rod bearing retainer (3)',(#17396));
#17336=PRODUCT_RELATED_PRODUCT_CATEGORY(
'Sealed Ball Bearing - 10 x 30 x 9 mm',
'Sealed Ball Bearing - 10 x 30 x 9 mm',(#17397));
#17337=PRODUCT_RELATED_PRODUCT_CATEGORY('Inner ring','Inner ring',(#17398));
#17338=PRODUCT_RELATED_PRODUCT_CATEGORY('Outer ring','Outer ring',(#17399));
#17339=PRODUCT_RELATED_PRODUCT_CATEGORY('Balls','Balls',(#17400));
#17340=PRODUCT_RELATED_PRODUCT_CATEGORY('Cage','Cage',(#17401));
#17341=PRODUCT_RELATED_PRODUCT_CATEGORY('Seals 2RS','Seals 2RS',(#17402));
#17342=PRODUCT_RELATED_PRODUCT_CATEGORY('Guided slider','Guided slider',
(#17403));
#17343=PRODUCT_RELATED_PRODUCT_CATEGORY('Specimen carriage',
'Specimen carriage',(#17404));
#17344=PRODUCT_RELATED_PRODUCT_CATEGORY('Specimen clamp jaw',
'Specimen clamp jaw',(#17405));
#17345=PRODUCT_RELATED_PRODUCT_CATEGORY('Slider pin','Slider pin',(#17406));
#17346=PRODUCT_RELATED_PRODUCT_CATEGORY('Pin spacer 2 mm',
'Pin spacer 2 mm',(#17407));
#17347=PRODUCT_RELATED_PRODUCT_CATEGORY('Pin spacer 4 mm (1)',
'Pin spacer 4 mm (1)',(#17408));
#17348=PRODUCT_RELATED_PRODUCT_CATEGORY('Pin keeper (1)',
'Pin keeper (1)',(#17409));
#17349=PRODUCT_RELATED_PRODUCT_CATEGORY(
'Flanged Linear Guide Carriage - 15 mm',
'Flanged Linear Guide Carriage - 15 mm',(#17410));
#17350=PRODUCT_RELATED_PRODUCT_CATEGORY('Block','Block',(#17411));
#17351=PRODUCT_RELATED_PRODUCT_CATEGORY('End cap +','End cap +',(#17412));
#17352=PRODUCT_RELATED_PRODUCT_CATEGORY('End cap','End cap',(#17413));
#17353=PRODUCT_RELATED_PRODUCT_CATEGORY('M5x14 Cap Screw',
'M5x14 Cap Screw',(#17414));
#17354=PRODUCT_RELATED_PRODUCT_CATEGORY('Flat Washer - M5',
'Flat Washer - M5',(#17415));
#17355=PRODUCT_RELATED_PRODUCT_CATEGORY('Cap Screw - M5x20',
'Cap Screw - M5x20',(#17416));
#17356=PRODUCT_RELATED_PRODUCT_CATEGORY('M4x10 Cap Screw',
'M4x10 Cap Screw',(#17417));
#17357=APPLICATION_PROTOCOL_DEFINITION('international standard',
'automotive_design',2009,#17358);
#17358=APPLICATION_CONTEXT(
'Core Data for Automotive Mechanical Design Process');
#17359=PRODUCT_CONTEXT('part definition',#17358,'mechanical');
#17360=PRODUCT('PAT-034','PAT-034',
'PAT-034',(#17359));
#17361=PRODUCT('Bearing and guide frame','Bearing and guide frame',
'Bearing and guide frame',(#17359));
#17362=PRODUCT('Base','Base','Base',(#17359));
#17363=PRODUCT('Bearing pedestal','Bearing pedestal','Bearing pedestal',
(#17359));
#17364=PRODUCT('Bearing bolt reducer','Bearing bolt reducer',
'Bearing bolt reducer',(#17359));
#17365=PRODUCT('Bearing bolt reducer (1)','Bearing bolt reducer (1)',
'Bearing bolt reducer (1)',(#17359));
#17366=PRODUCT('Bearing pedestal (1)','Bearing pedestal (1)',
'Bearing pedestal (1)',(#17359));
#17367=PRODUCT('Bearing bolt reducer (2)','Bearing bolt reducer (2)',
'Bearing bolt reducer (2)',(#17359));
#17368=PRODUCT('Bearing bolt reducer (3)','Bearing bolt reducer (3)',
'Bearing bolt reducer (3)',(#17359));
#17369=PRODUCT('Rail pedestal','Rail pedestal','Rail pedestal',(#17359));
#17370=PRODUCT('Foot strip','Foot strip','Foot strip',(#17359));
#17371=PRODUCT('Foot strip (1)','Foot strip (1)','Foot strip (1)',(#17359));
#17372=PRODUCT('Pillow Block Bearing - 20 mm Bore',
'Pillow Block Bearing - 20 mm Bore','Pillow Block Bearing - 20 mm Bore',
(#17359));
#17373=PRODUCT('Housing','Housing','Housing',(#17359));
#17374=PRODUCT('Insert bearing','Insert bearing','Insert bearing',(#17359));
#17375=PRODUCT('Flat Washer - M8','Flat Washer - M8','Flat Washer - M8',
(#17359));
#17376=PRODUCT('M8x25 Bolt','M8x25 Bolt','M8x25 Bolt',(#17359));
#17377=PRODUCT('Linear Guide Rail - 15 mm, 220 mm Long',
'Linear Guide Rail - 15 mm, 220 mm Long',
'Linear Guide Rail - 15 mm, 220 mm Long',(#17359));
#17378=PRODUCT('Cap Screw - M4x16','Cap Screw - M4x16',
'Cap Screw - M4x16',(#17359));
#17379=PRODUCT('Flywheel and crank','Flywheel and crank',
'Flywheel and crank',(#17359));
#17380=PRODUCT('Flywheel shaft','Flywheel shaft','Flywheel shaft',(#17359));
#17381=PRODUCT('Shaft collar','Shaft collar','Shaft collar',(#17359));
#17382=PRODUCT('Shaft collar (1)','Shaft collar (1)','Shaft collar (1)',(#17359));
#17383=PRODUCT('Rear bearing spacer','Rear bearing spacer',
'Rear bearing spacer',(#17359));
#17384=PRODUCT('Flywheel','Flywheel','Flywheel',(#17359));
#17385=PRODUCT('Crank pin','Crank pin','Crank pin',(#17359));
#17386=PRODUCT('Pin spacer 15 mm','Pin spacer 15 mm','Pin spacer 15 mm',
(#17359));
#17387=PRODUCT('Pin spacer 4 mm','Pin spacer 4 mm','Pin spacer 4 mm',(#17359));
#17388=PRODUCT('Pin keeper','Pin keeper','Pin keeper',(#17359));
#17389=PRODUCT('Key 6x6x20','Key 6x6x20','Key 6x6x20',(#17359));
#17390=PRODUCT('Socket Set Screw - M5x8','Socket Set Screw - M5x8',
'Socket Set Screw - M5x8',(#17359));
#17391=PRODUCT('Connecting rod (1)','Connecting rod (1)','Connecting rod (1)',(#17359));
#17392=PRODUCT('Connecting rod','Connecting rod','Connecting rod',(#17359));
#17393=PRODUCT('Rod bearing retainer','Rod bearing retainer',
'Rod bearing retainer',(#17359));
#17394=PRODUCT('Rod bearing retainer (1)','Rod bearing retainer (1)',
'Rod bearing retainer (1)',(#17359));
#17395=PRODUCT('Rod bearing retainer (2)','Rod bearing retainer (2)',
'Rod bearing retainer (2)',(#17359));
#17396=PRODUCT('Rod bearing retainer (3)','Rod bearing retainer (3)',
'Rod bearing retainer (3)',(#17359));
#17397=PRODUCT('Sealed Ball Bearing - 10 x 30 x 9 mm',
'Sealed Ball Bearing - 10 x 30 x 9 mm',
'Sealed Ball Bearing - 10 x 30 x 9 mm',(#17359));
#17398=PRODUCT('Inner ring','Inner ring','Inner ring',(#17359));
#17399=PRODUCT('Outer ring','Outer ring','Outer ring',(#17359));
#17400=PRODUCT('Balls','Balls','Balls',(#17359));
#17401=PRODUCT('Cage','Cage','Cage',(#17359));
#17402=PRODUCT('Seals 2RS','Seals 2RS','Seals 2RS',(#17359));
#17403=PRODUCT('Guided slider','Guided slider','Guided slider',(#17359));
#17404=PRODUCT('Specimen carriage','Specimen carriage',
'Specimen carriage',(#17359));
#17405=PRODUCT('Specimen clamp jaw','Specimen clamp jaw',
'Specimen clamp jaw',(#17359));
#17406=PRODUCT('Slider pin','Slider pin','Slider pin',(#17359));
#17407=PRODUCT('Pin spacer 2 mm','Pin spacer 2 mm','Pin spacer 2 mm',(#17359));
#17408=PRODUCT('Pin spacer 4 mm (1)','Pin spacer 4 mm (1)',
'Pin spacer 4 mm (1)',(#17359));
#17409=PRODUCT('Pin keeper (1)','Pin keeper (1)','Pin keeper (1)',(#17359));
#17410=PRODUCT('Flanged Linear Guide Carriage - 15 mm',
'Flanged Linear Guide Carriage - 15 mm',
'Flanged Linear Guide Carriage - 15 mm',(#17359));
#17411=PRODUCT('Block','Block','Block',(#17359));
#17412=PRODUCT('End cap +','End cap +','End cap +',(#17359));
#17413=PRODUCT('End cap','End cap','End cap',(#17359));
#17414=PRODUCT('M5x14 Cap Screw','M5x14 Cap Screw','M5x14 Cap Screw',(#17359));
#17415=PRODUCT('Flat Washer - M5','Flat Washer - M5','Flat Washer - M5',
(#17359));
#17416=PRODUCT('Cap Screw - M5x20','Cap Screw - M5x20',
'Cap Screw - M5x20',(#17359));
#17417=PRODUCT('M4x10 Cap Screw','M4x10 Cap Screw','M4x10 Cap Screw',(#17359));
#17418=PRESENTATION_STYLE_ASSIGNMENT((#17424));
#17419=PRESENTATION_STYLE_ASSIGNMENT((#17425));
#17420=PRESENTATION_STYLE_ASSIGNMENT((#17426));
#17421=PRESENTATION_STYLE_ASSIGNMENT((#17427));
#17422=PRESENTATION_STYLE_ASSIGNMENT((#17428));
#17423=PRESENTATION_STYLE_ASSIGNMENT((#17429));
#17424=SURFACE_STYLE_USAGE(.BOTH.,#17430);
#17425=SURFACE_STYLE_USAGE(.BOTH.,#17431);
#17426=SURFACE_STYLE_USAGE(.BOTH.,#17432);
#17427=SURFACE_STYLE_USAGE(.BOTH.,#17433);
#17428=SURFACE_STYLE_USAGE(.BOTH.,#17434);
#17429=SURFACE_STYLE_USAGE(.BOTH.,#17435);
#17430=SURFACE_SIDE_STYLE('',(#17436));
#17431=SURFACE_SIDE_STYLE('',(#17437));
#17432=SURFACE_SIDE_STYLE('',(#17438));
#17433=SURFACE_SIDE_STYLE('',(#17439));
#17434=SURFACE_SIDE_STYLE('',(#17440));
#17435=SURFACE_SIDE_STYLE('',(#17441));
#17436=SURFACE_STYLE_FILL_AREA(#17442);
#17437=SURFACE_STYLE_FILL_AREA(#17443);
#17438=SURFACE_STYLE_FILL_AREA(#17444);
#17439=SURFACE_STYLE_FILL_AREA(#17445);
#17440=SURFACE_STYLE_FILL_AREA(#17446);
#17441=SURFACE_STYLE_FILL_AREA(#17447);
#17442=FILL_AREA_STYLE('Steel - Satin',(#17448));
#17443=FILL_AREA_STYLE('CAD Library Painted - Deep blue',(#17449));
#17444=FILL_AREA_STYLE('CAD Library Painted - Steel gray',(#17450));
#17445=FILL_AREA_STYLE('CAD Library Painted - Graphite',(#17451));
#17446=FILL_AREA_STYLE('CAD Library Painted - Engineering blue',(#17452));
#17447=FILL_AREA_STYLE('CAD Library Painted - Light blue',(#17453));
#17448=FILL_AREA_STYLE_COLOUR('Steel - Satin',#17454);
#17449=FILL_AREA_STYLE_COLOUR('CAD Library Painted - Deep blue',#17455);
#17450=FILL_AREA_STYLE_COLOUR('CAD Library Painted - Steel gray',#17456);
#17451=FILL_AREA_STYLE_COLOUR('CAD Library Painted - Graphite',#17457);
#17452=FILL_AREA_STYLE_COLOUR('CAD Library Painted - Engineering blue',
#17458);
#17453=FILL_AREA_STYLE_COLOUR('CAD Library Painted - Light blue',#17459);
#17454=COLOUR_RGB('Steel - Satin',0.627450980392157,0.627450980392157,0.627450980392157);
#17455=COLOUR_RGB('CAD Library Painted - Deep blue',0.0784313725490196,
0.203921568627451,0.349019607843137);
#17456=COLOUR_RGB('CAD Library Painted - Steel gray',0.592156862745098,
0.631372549019608,0.67843137254902);
#17457=COLOUR_RGB('CAD Library Painted - Graphite',0.168627450980392,0.192156862745098,
0.231372549019608);
#17458=COLOUR_RGB('CAD Library Painted - Engineering blue',0.12156862745098,
0.356862745098039,0.6);
#17459=COLOUR_RGB('CAD Library Painted - Light blue',0.286274509803922,
0.552941176470588,0.780392156862745);
#17460=COLOUR_RGB('Dark Blue',0.08,0.2,0.34);
#17461=FILL_AREA_STYLE_COLOUR('',#17460);
#17462=FILL_AREA_STYLE('',(#17461));
#17463=SURFACE_STYLE_FILL_AREA(#17462);
#17464=SURFACE_SIDE_STYLE('',(#17463));
#17465=SURFACE_STYLE_USAGE(.BOTH.,#17464);
#17466=PRESENTATION_STYLE_ASSIGNMENT((#17465));
#17467=COLOUR_RGB('Light Blue',0.38,0.62,0.78);
#17468=FILL_AREA_STYLE_COLOUR('',#17467);
#17469=FILL_AREA_STYLE('',(#17468));
#17470=SURFACE_STYLE_FILL_AREA(#17469);
#17471=SURFACE_SIDE_STYLE('',(#17470));
#17472=SURFACE_STYLE_USAGE(.BOTH.,#17471);
#17473=PRESENTATION_STYLE_ASSIGNMENT((#17472));
#17474=COLOUR_RGB('Sky Blue',0.24,0.69,0.87);
#17475=FILL_AREA_STYLE_COLOUR('',#17474);
#17476=FILL_AREA_STYLE('',(#17475));
#17477=SURFACE_STYLE_FILL_AREA(#17476);
#17478=SURFACE_SIDE_STYLE('',(#17477));
#17479=SURFACE_STYLE_USAGE(.BOTH.,#17478);
#17480=PRESENTATION_STYLE_ASSIGNMENT((#17479));
#17481=COLOUR_RGB('Grey',0.48,0.52,0.57);
#17482=FILL_AREA_STYLE_COLOUR('',#17481);
#17483=FILL_AREA_STYLE('',(#17482));
#17484=SURFACE_STYLE_FILL_AREA(#17483);
#17485=SURFACE_SIDE_STYLE('',(#17484));
#17486=SURFACE_STYLE_USAGE(.BOTH.,#17485);
#17487=PRESENTATION_STYLE_ASSIGNMENT((#17486));
#17488=COLOUR_RGB('Black',0.12,0.14,0.17);
#17489=FILL_AREA_STYLE_COLOUR('',#17488);
#17490=FILL_AREA_STYLE('',(#17489));
#17491=SURFACE_STYLE_FILL_AREA(#17490);
#17492=SURFACE_SIDE_STYLE('',(#17491));
#17493=SURFACE_STYLE_USAGE(.BOTH.,#17492);
#17494=PRESENTATION_STYLE_ASSIGNMENT((#17493));
#17495=COLOUR_RGB('Off White',0.89,0.88,0.83);
#17496=FILL_AREA_STYLE_COLOUR('',#17495);
#17497=FILL_AREA_STYLE('',(#17496));
#17498=SURFACE_STYLE_FILL_AREA(#17497);
#17499=SURFACE_SIDE_STYLE('',(#17498));
#17500=SURFACE_STYLE_USAGE(.BOTH.,#17499);
#17501=PRESENTATION_STYLE_ASSIGNMENT((#17500));
ENDSEC;
END-ISO-10303-21;
